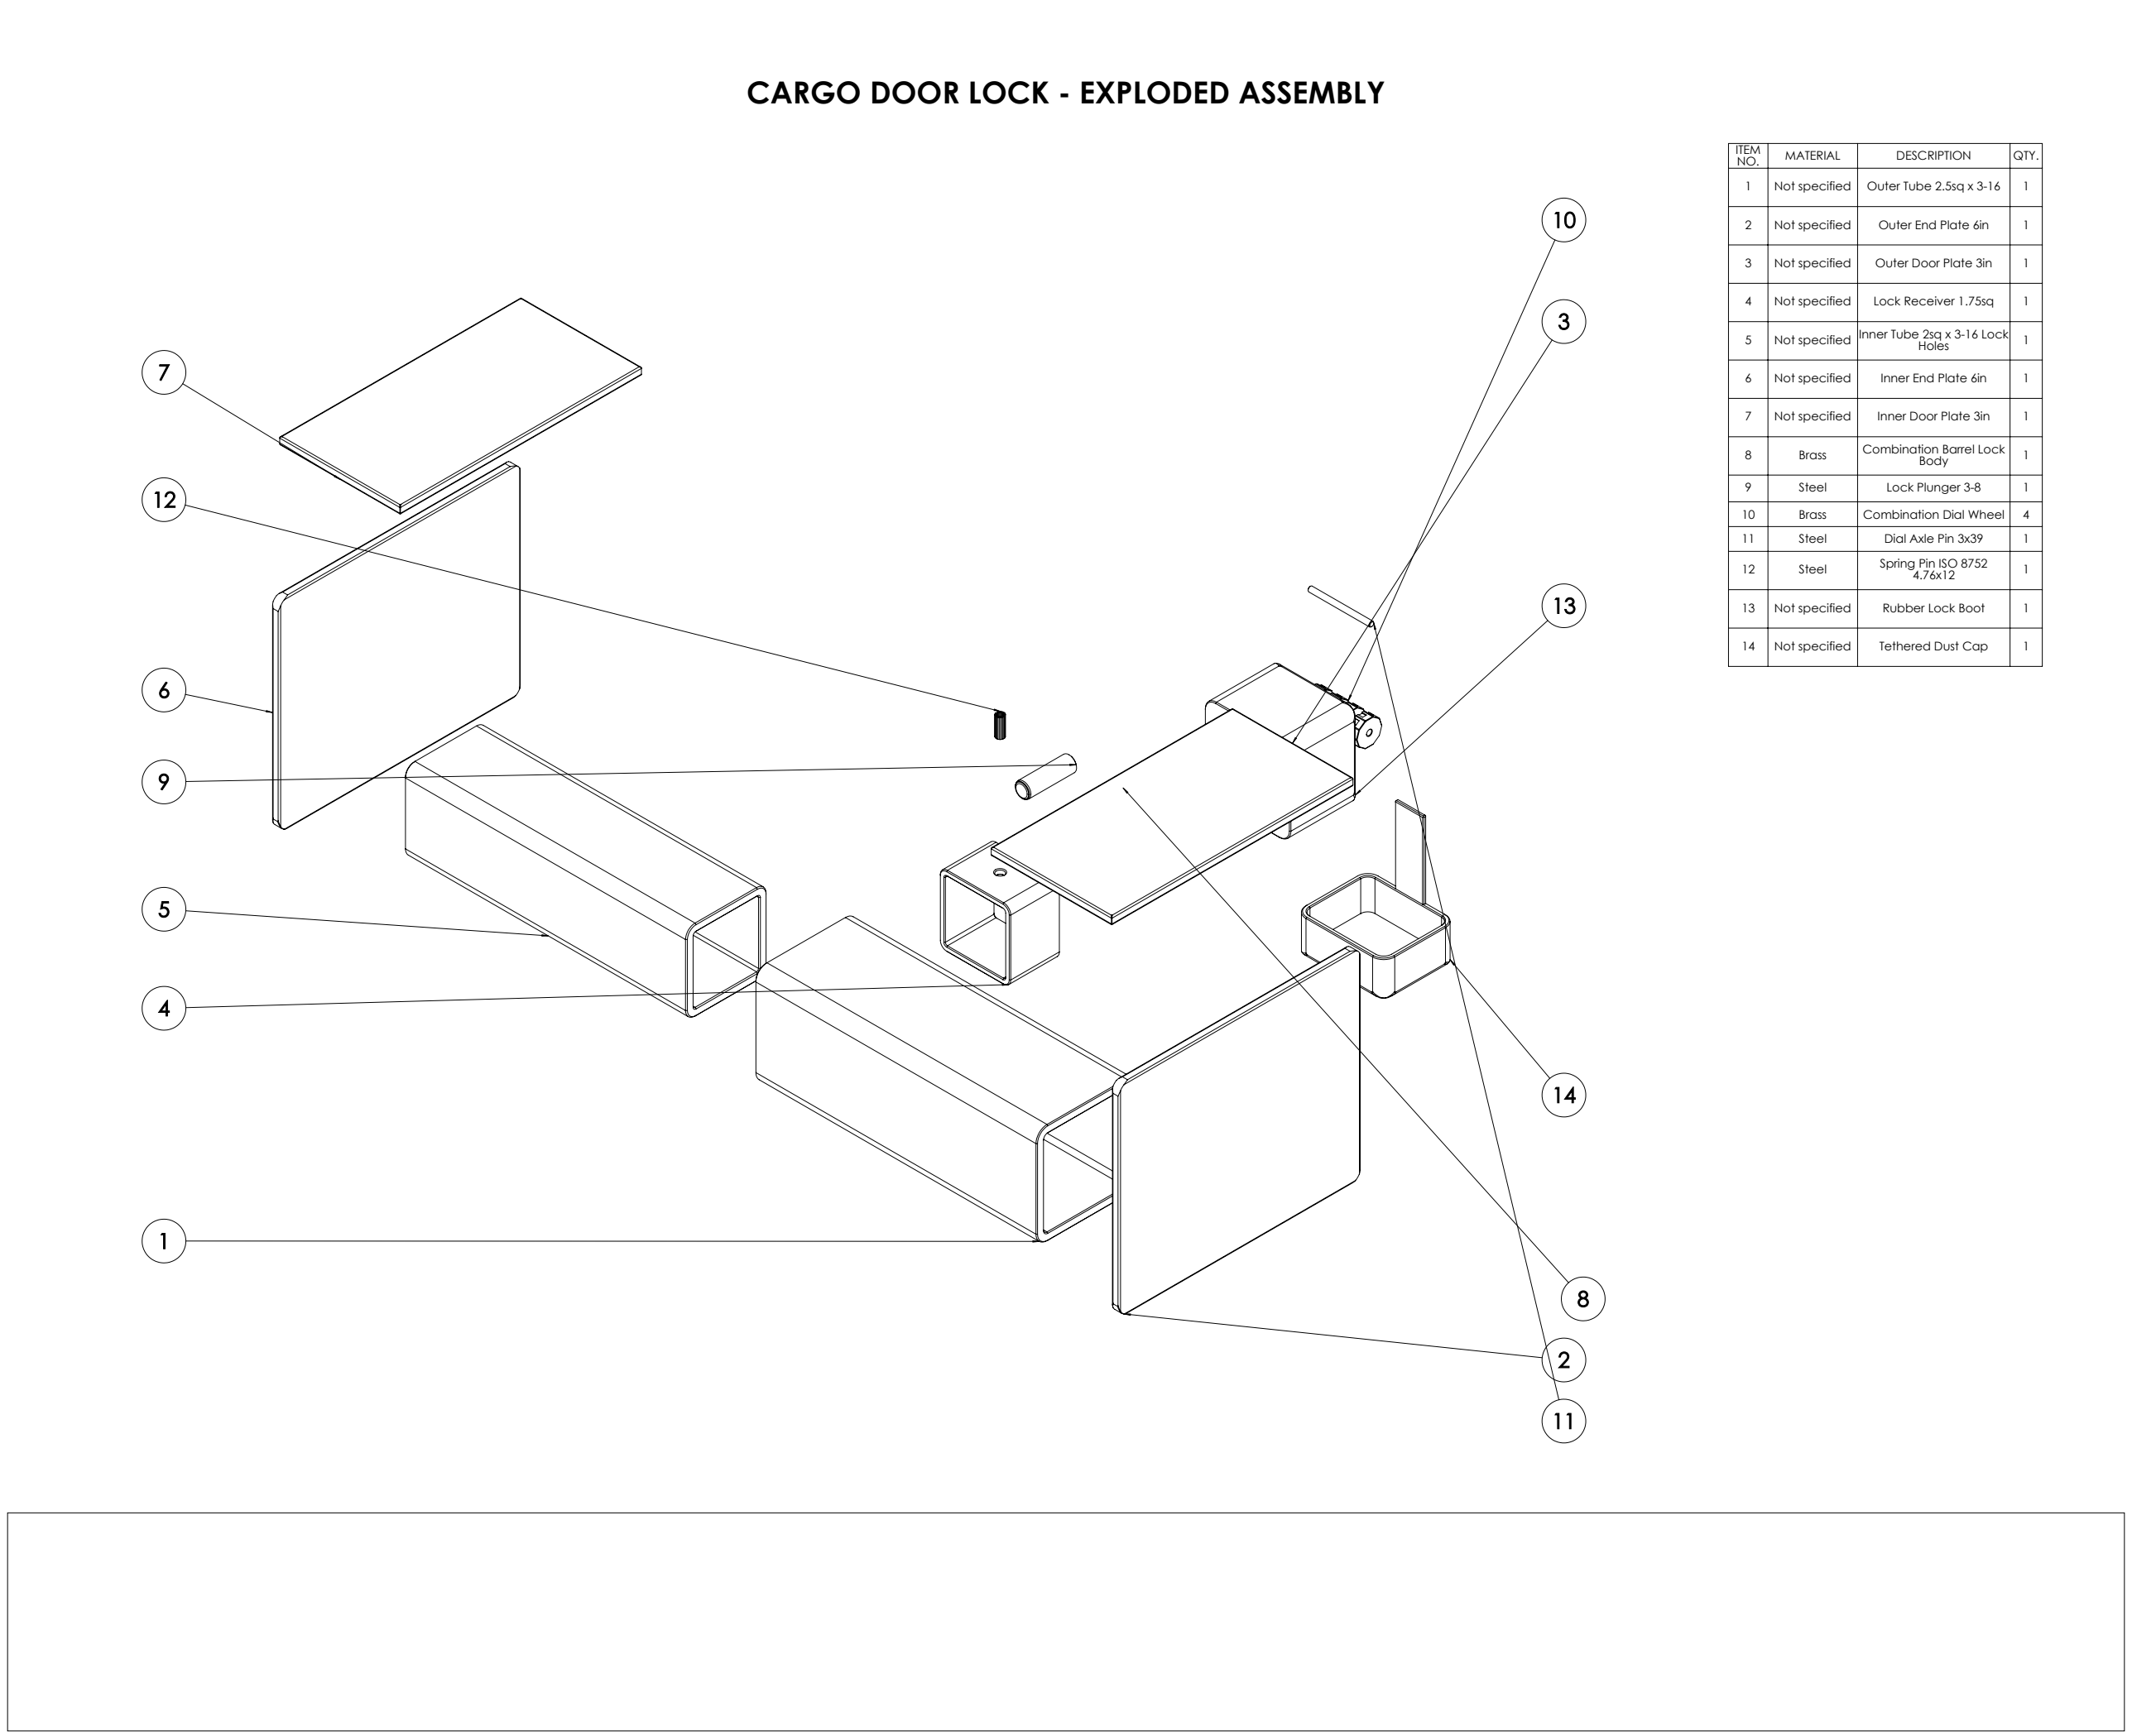
ISO-10303-21;
HEADER;
/* Generated by software containing ST-Developer
 * from STEP Tools, Inc. (www.steptools.com) 
 */

FILE_DESCRIPTION(
/* description */ (''),
/* implementation_level */ '2;1');

FILE_NAME(
/* name */ 'MAS-499',
/* time_stamp */ '2026-10-25T01:30:15-07:00',
/* author */ (''),
/* organization */ (''),
/* preprocessor_version */ 'ST-DEVELOPER v20.2',
/* originating_system */ 'Autodesk Translation Framework v15.15.0.0',
/* authorisation */ '');

FILE_SCHEMA (('AUTOMOTIVE_DESIGN { 1 0 10303 214 3 1 1 }'));
ENDSEC;

DATA;
#10=MECHANICAL_DESIGN_GEOMETRIC_PRESENTATION_REPRESENTATION('',(#563,#564,
#565,#566,#567,#568,#569,#570,#571,#572,#573,#574,#575,#576),#32309);
#11=ITEM_DEFINED_TRANSFORMATION($,$,#13974,#14987);
#12=ITEM_DEFINED_TRANSFORMATION($,$,#14060,#14988);
#13=ITEM_DEFINED_TRANSFORMATION($,$,#14095,#14989);
#14=ITEM_DEFINED_TRANSFORMATION($,$,#14114,#14990);
#15=ITEM_DEFINED_TRANSFORMATION($,$,#14204,#14991);
#16=ITEM_DEFINED_TRANSFORMATION($,$,#14378,#14992);
#17=ITEM_DEFINED_TRANSFORMATION($,$,#14413,#14993);
#18=ITEM_DEFINED_TRANSFORMATION($,$,#14432,#14994);
#19=ITEM_DEFINED_TRANSFORMATION($,$,#14610,#14995);
#20=ITEM_DEFINED_TRANSFORMATION($,$,#14627,#14996);
#21=ITEM_DEFINED_TRANSFORMATION($,$,#14637,#14997);
#22=ITEM_DEFINED_TRANSFORMATION($,$,#14690,#14998);
#23=ITEM_DEFINED_TRANSFORMATION($,$,#14802,#14999);
#24=ITEM_DEFINED_TRANSFORMATION($,$,#14889,#15000);
#25=ITEM_DEFINED_TRANSFORMATION($,$,#14889,#15001);
#26=ITEM_DEFINED_TRANSFORMATION($,$,#14889,#15002);
#27=ITEM_DEFINED_TRANSFORMATION($,$,#14889,#15003);
#28=(
REPRESENTATION_RELATIONSHIP($,$,#32362,#32361)
REPRESENTATION_RELATIONSHIP_WITH_TRANSFORMATION(#11)
SHAPE_REPRESENTATION_RELATIONSHIP()
);
#29=(
REPRESENTATION_RELATIONSHIP($,$,#32363,#32361)
REPRESENTATION_RELATIONSHIP_WITH_TRANSFORMATION(#12)
SHAPE_REPRESENTATION_RELATIONSHIP()
);
#30=(
REPRESENTATION_RELATIONSHIP($,$,#32364,#32361)
REPRESENTATION_RELATIONSHIP_WITH_TRANSFORMATION(#13)
SHAPE_REPRESENTATION_RELATIONSHIP()
);
#31=(
REPRESENTATION_RELATIONSHIP($,$,#32365,#32361)
REPRESENTATION_RELATIONSHIP_WITH_TRANSFORMATION(#14)
SHAPE_REPRESENTATION_RELATIONSHIP()
);
#32=(
REPRESENTATION_RELATIONSHIP($,$,#32366,#32361)
REPRESENTATION_RELATIONSHIP_WITH_TRANSFORMATION(#15)
SHAPE_REPRESENTATION_RELATIONSHIP()
);
#33=(
REPRESENTATION_RELATIONSHIP($,$,#32367,#32361)
REPRESENTATION_RELATIONSHIP_WITH_TRANSFORMATION(#16)
SHAPE_REPRESENTATION_RELATIONSHIP()
);
#34=(
REPRESENTATION_RELATIONSHIP($,$,#32368,#32361)
REPRESENTATION_RELATIONSHIP_WITH_TRANSFORMATION(#17)
SHAPE_REPRESENTATION_RELATIONSHIP()
);
#35=(
REPRESENTATION_RELATIONSHIP($,$,#32369,#32361)
REPRESENTATION_RELATIONSHIP_WITH_TRANSFORMATION(#18)
SHAPE_REPRESENTATION_RELATIONSHIP()
);
#36=(
REPRESENTATION_RELATIONSHIP($,$,#32370,#32361)
REPRESENTATION_RELATIONSHIP_WITH_TRANSFORMATION(#19)
SHAPE_REPRESENTATION_RELATIONSHIP()
);
#37=(
REPRESENTATION_RELATIONSHIP($,$,#32371,#32361)
REPRESENTATION_RELATIONSHIP_WITH_TRANSFORMATION(#20)
SHAPE_REPRESENTATION_RELATIONSHIP()
);
#38=(
REPRESENTATION_RELATIONSHIP($,$,#32372,#32361)
REPRESENTATION_RELATIONSHIP_WITH_TRANSFORMATION(#21)
SHAPE_REPRESENTATION_RELATIONSHIP()
);
#39=(
REPRESENTATION_RELATIONSHIP($,$,#32373,#32361)
REPRESENTATION_RELATIONSHIP_WITH_TRANSFORMATION(#22)
SHAPE_REPRESENTATION_RELATIONSHIP()
);
#40=(
REPRESENTATION_RELATIONSHIP($,$,#32374,#32361)
REPRESENTATION_RELATIONSHIP_WITH_TRANSFORMATION(#23)
SHAPE_REPRESENTATION_RELATIONSHIP()
);
#41=(
REPRESENTATION_RELATIONSHIP($,$,#32375,#32361)
REPRESENTATION_RELATIONSHIP_WITH_TRANSFORMATION(#24)
SHAPE_REPRESENTATION_RELATIONSHIP()
);
#42=(
REPRESENTATION_RELATIONSHIP($,$,#32375,#32361)
REPRESENTATION_RELATIONSHIP_WITH_TRANSFORMATION(#25)
SHAPE_REPRESENTATION_RELATIONSHIP()
);
#43=(
REPRESENTATION_RELATIONSHIP($,$,#32375,#32361)
REPRESENTATION_RELATIONSHIP_WITH_TRANSFORMATION(#26)
SHAPE_REPRESENTATION_RELATIONSHIP()
);
#44=(
REPRESENTATION_RELATIONSHIP($,$,#32375,#32361)
REPRESENTATION_RELATIONSHIP_WITH_TRANSFORMATION(#27)
SHAPE_REPRESENTATION_RELATIONSHIP()
);
#45=CONTEXT_DEPENDENT_SHAPE_REPRESENTATION(#28,#32344);
#46=CONTEXT_DEPENDENT_SHAPE_REPRESENTATION(#29,#32345);
#47=CONTEXT_DEPENDENT_SHAPE_REPRESENTATION(#30,#32346);
#48=CONTEXT_DEPENDENT_SHAPE_REPRESENTATION(#31,#32347);
#49=CONTEXT_DEPENDENT_SHAPE_REPRESENTATION(#32,#32348);
#50=CONTEXT_DEPENDENT_SHAPE_REPRESENTATION(#33,#32349);
#51=CONTEXT_DEPENDENT_SHAPE_REPRESENTATION(#34,#32350);
#52=CONTEXT_DEPENDENT_SHAPE_REPRESENTATION(#35,#32351);
#53=CONTEXT_DEPENDENT_SHAPE_REPRESENTATION(#36,#32352);
#54=CONTEXT_DEPENDENT_SHAPE_REPRESENTATION(#37,#32353);
#55=CONTEXT_DEPENDENT_SHAPE_REPRESENTATION(#38,#32354);
#56=CONTEXT_DEPENDENT_SHAPE_REPRESENTATION(#39,#32355);
#57=CONTEXT_DEPENDENT_SHAPE_REPRESENTATION(#40,#32356);
#58=CONTEXT_DEPENDENT_SHAPE_REPRESENTATION(#41,#32357);
#59=CONTEXT_DEPENDENT_SHAPE_REPRESENTATION(#42,#32358);
#60=CONTEXT_DEPENDENT_SHAPE_REPRESENTATION(#43,#32359);
#61=CONTEXT_DEPENDENT_SHAPE_REPRESENTATION(#44,#32360);
#62=NEXT_ASSEMBLY_USAGE_OCCURRENCE('01_Outer_Tube_2.5sq_x_3-16:2',
'01_Outer_Tube_2.5sq_x_3-16:2','01_Outer_Tube_2.5sq_x_3-16:2',#32377,#32378,
'01_Outer_Tube_2.5sq_x_3-16:2');
#63=NEXT_ASSEMBLY_USAGE_OCCURRENCE('02_Outer_End_Plate_6in:2',
'02_Outer_End_Plate_6in:2','02_Outer_End_Plate_6in:2',#32377,#32379,
'02_Outer_End_Plate_6in:2');
#64=NEXT_ASSEMBLY_USAGE_OCCURRENCE('03_Outer_Door_Plate_3in:2',
'03_Outer_Door_Plate_3in:2','03_Outer_Door_Plate_3in:2',#32377,#32380,
'03_Outer_Door_Plate_3in:2');
#65=NEXT_ASSEMBLY_USAGE_OCCURRENCE('04_Lock_Receiver_1.75sq:2',
'04_Lock_Receiver_1.75sq:2','04_Lock_Receiver_1.75sq:2',#32377,#32381,
'04_Lock_Receiver_1.75sq:2');
#66=NEXT_ASSEMBLY_USAGE_OCCURRENCE(
'05_Inner_Tube_2sq_x_3-16_Lock_Holes:2',
'05_Inner_Tube_2sq_x_3-16_Lock_Holes:2',
'05_Inner_Tube_2sq_x_3-16_Lock_Holes:2',#32377,#32382,
'05_Inner_Tube_2sq_x_3-16_Lock_Holes:2');
#67=NEXT_ASSEMBLY_USAGE_OCCURRENCE('06_Inner_End_Plate_6in:2',
'06_Inner_End_Plate_6in:2','06_Inner_End_Plate_6in:2',#32377,#32383,
'06_Inner_End_Plate_6in:2');
#68=NEXT_ASSEMBLY_USAGE_OCCURRENCE('07_Inner_Door_Plate_3in:2',
'07_Inner_Door_Plate_3in:2','07_Inner_Door_Plate_3in:2',#32377,#32384,
'07_Inner_Door_Plate_3in:2');
#69=NEXT_ASSEMBLY_USAGE_OCCURRENCE('08_Combination_Barrel_Lock_Body:2',
'08_Combination_Barrel_Lock_Body:2','08_Combination_Barrel_Lock_Body:2',
#32377,#32385,'08_Combination_Barrel_Lock_Body:2');
#70=NEXT_ASSEMBLY_USAGE_OCCURRENCE('09_Lock_Plunger_3-8:2',
'09_Lock_Plunger_3-8:2','09_Lock_Plunger_3-8:2',#32377,#32386,
'09_Lock_Plunger_3-8:2');
#71=NEXT_ASSEMBLY_USAGE_OCCURRENCE('11_Dial_Axle_Pin_3x39:2',
'11_Dial_Axle_Pin_3x39:2','11_Dial_Axle_Pin_3x39:2',#32377,#32387,
'11_Dial_Axle_Pin_3x39:2');
#72=NEXT_ASSEMBLY_USAGE_OCCURRENCE('12_Spring_Pin_ISO_8752_4.76x12:2',
'12_Spring_Pin_ISO_8752_4.76x12:2','12_Spring_Pin_ISO_8752_4.76x12:2',#32377,
#32388,'12_Spring_Pin_ISO_8752_4.76x12:2');
#73=NEXT_ASSEMBLY_USAGE_OCCURRENCE('13_Rubber_Lock_Boot:2',
'13_Rubber_Lock_Boot:2','13_Rubber_Lock_Boot:2',#32377,#32389,
'13_Rubber_Lock_Boot:2');
#74=NEXT_ASSEMBLY_USAGE_OCCURRENCE('14_Tethered_Dust_Cap:2',
'14_Tethered_Dust_Cap:2','14_Tethered_Dust_Cap:2',#32377,#32390,
'14_Tethered_Dust_Cap:2');
#75=NEXT_ASSEMBLY_USAGE_OCCURRENCE('10_Combination_Dial_Wheel:2',
'10_Combination_Dial_Wheel:2','10_Combination_Dial_Wheel:2',#32377,#32391,
'10_Combination_Dial_Wheel:2');
#76=NEXT_ASSEMBLY_USAGE_OCCURRENCE('10_Combination_Dial_Wheel:3',
'10_Combination_Dial_Wheel:3','10_Combination_Dial_Wheel:3',#32377,#32391,
'10_Combination_Dial_Wheel:3');
#77=NEXT_ASSEMBLY_USAGE_OCCURRENCE('10_Combination_Dial_Wheel:4',
'10_Combination_Dial_Wheel:4','10_Combination_Dial_Wheel:4',#32377,#32391,
'10_Combination_Dial_Wheel:4');
#78=NEXT_ASSEMBLY_USAGE_OCCURRENCE('10_Combination_Dial_Wheel:5',
'10_Combination_Dial_Wheel:5','10_Combination_Dial_Wheel:5',#32377,#32391,
'10_Combination_Dial_Wheel:5');
#79=ELLIPSE('',#14443,12.7279220613578,8.99999999999999);
#80=ELLIPSE('',#14447,12.7279220613579,9.);
#81=ELLIPSE('',#14470,12.7279220613578,9.);
#82=ELLIPSE('',#14474,12.7279220613578,9.);
#83=(
BOUNDED_CURVE()
B_SPLINE_CURVE(2,(#25941,#25942,#25943),.UNSPECIFIED.,.F.,.F.)
B_SPLINE_CURVE_WITH_KNOTS((3,3),(0.,0.083454512499127),.UNSPECIFIED.)
CURVE()
GEOMETRIC_REPRESENTATION_ITEM()
RATIONAL_B_SPLINE_CURVE((1.,1.00072968826169,1.))
REPRESENTATION_ITEM('')
);
#84=(
BOUNDED_CURVE()
B_SPLINE_CURVE(2,(#25958,#25959,#25960),.UNSPECIFIED.,.F.,.F.)
B_SPLINE_CURVE_WITH_KNOTS((3,3),(0.,0.0834545124991277),.UNSPECIFIED.)
CURVE()
GEOMETRIC_REPRESENTATION_ITEM()
RATIONAL_B_SPLINE_CURVE((1.,1.00072968826163,1.))
REPRESENTATION_ITEM('')
);
#85=(
BOUNDED_CURVE()
B_SPLINE_CURVE(2,(#26021,#26022,#26023),.UNSPECIFIED.,.F.,.F.)
B_SPLINE_CURVE_WITH_KNOTS((3,3),(0.,0.0834545124991279),.UNSPECIFIED.)
CURVE()
GEOMETRIC_REPRESENTATION_ITEM()
RATIONAL_B_SPLINE_CURVE((1.,1.00072968826024,1.))
REPRESENTATION_ITEM('')
);
#86=(
BOUNDED_CURVE()
B_SPLINE_CURVE(2,(#26038,#26039,#26040),.UNSPECIFIED.,.F.,.F.)
B_SPLINE_CURVE_WITH_KNOTS((3,3),(0.,0.083454512499128),.UNSPECIFIED.)
CURVE()
GEOMETRIC_REPRESENTATION_ITEM()
RATIONAL_B_SPLINE_CURVE((1.,1.0007296882565,1.))
REPRESENTATION_ITEM('')
);
#87=(
BOUNDED_CURVE()
B_SPLINE_CURVE(3,(#30768,#30769,#30770,#30771,#30772,#30773,#30774,#30775,
#30776,#30777,#30778,#30779),.UNSPECIFIED.,.F.,.F.)
B_SPLINE_CURVE_WITH_KNOTS((4,2,2,2,2,4),(0.000100085581199306,0.11804875878528,
0.236101413685198,0.384034650166034,0.497829447458985,0.511841573844537),
 .UNSPECIFIED.)
CURVE()
GEOMETRIC_REPRESENTATION_ITEM()
RATIONAL_B_SPLINE_CURVE((1.,1.,1.,1.,1.,1.,1.,1.,1.,1.,1.,1.))
REPRESENTATION_ITEM('')
);
#88=B_SPLINE_CURVE_WITH_KNOTS('',3,(#18634,#18635,#18636,#18637,#18638,
#18639,#18640,#18641,#18642,#18643,#18644,#18645,#18646,#18647,#18648,#18649,
#18650,#18651,#18652,#18653,#18654,#18655,#18656,#18657,#18658,#18659,#18660,
#18661,#18662,#18663,#18664,#18665,#18666,#18667,#18668,#18669,#18670,#18671,
#18672,#18673,#18674,#18675,#18676,#18677,#18678,#18679,#18680,#18681,#18682,
#18683,#18684,#18685,#18686,#18687,#18688,#18689,#18690,#18691,#18692,#18693,
#18694,#18695,#18696,#18697,#18698,#18699,#18700,#18701,#18702,#18703,#18704,
#18705,#18706,#18707,#18708,#18709,#18710,#18711,#18712,#18713,#18714,#18715),
 .UNSPECIFIED.,.F.,.F.,(4,3,3,3,3,3,3,3,3,3,3,3,3,3,3,3,3,3,3,3,3,3,3,3,
3,3,3,4),(0.,0.0295705059520471,0.06051594873034,0.0926038163611335,0.126139587235275,
0.161619669140697,0.19997110729461,0.243460414926569,0.31097643988682,0.354040412393894,
0.394412886619275,0.429686040742309,0.462833625340497,0.494651029781358,
0.527129557828368,0.560643520110525,0.596019930687279,0.634095034705998,
0.676984118479283,0.757738088859462,0.799051739150417,0.836280907609681,
0.871099049046634,0.903485295335691,0.934889314251083,0.965468175632905,
0.995091329104342,1.),.UNSPECIFIED.);
#89=B_SPLINE_CURVE_WITH_KNOTS('',3,(#18717,#18718,#18719,#18720),
 .UNSPECIFIED.,.F.,.F.,(4,4),(-1.,0.),.UNSPECIFIED.);
#90=B_SPLINE_CURVE_WITH_KNOTS('',3,(#18722,#18723,#18724,#18725,#18726,
#18727,#18728,#18729,#18730,#18731,#18732,#18733,#18734,#18735,#18736,#18737,
#18738,#18739,#18740,#18741,#18742,#18743,#18744,#18745,#18746,#18747,#18748,
#18749,#18750,#18751,#18752,#18753,#18754,#18755,#18756,#18757,#18758,#18759,
#18760,#18761,#18762,#18763,#18764,#18765,#18766,#18767,#18768,#18769,#18770,
#18771,#18772,#18773),.UNSPECIFIED.,.F.,.F.,(4,3,3,3,3,3,3,3,3,3,3,3,3,
3,3,3,3,4),(0.,0.0499444618814776,0.102213228769125,0.161337745851018,0.226027786935006,
0.32277431356813,0.388018393772404,0.444871191794535,0.498045966144255,
0.551308035192963,0.608971249854249,0.676370629164652,0.757277971873489,
0.819640070739892,0.87628793152519,0.929442915859961,0.979183143018599,
1.),.UNSPECIFIED.);
#91=B_SPLINE_CURVE_WITH_KNOTS('',3,(#18813,#18814,#18815,#18816,#18817,
#18818,#18819,#18820,#18821,#18822,#18823,#18824,#18825,#18826,#18827,#18828,
#18829,#18830,#18831,#18832,#18833,#18834,#18835,#18836,#18837,#18838,#18839,
#18840,#18841,#18842,#18843,#18844,#18845,#18846,#18847,#18848,#18849,#18850,
#18851,#18852,#18853,#18854,#18855,#18856,#18857,#18858,#18859,#18860,#18861,
#18862,#18863,#18864),.UNSPECIFIED.,.F.,.F.,(4,3,3,3,3,3,3,3,3,3,3,3,3,
3,3,3,3,4),(0.,0.0499441833889704,0.102212663354794,0.161336814770105,0.226026300658832,
0.322773013076478,0.388016980146257,0.444869605985199,0.498043900535364,
0.551305760953485,0.608968431114082,0.676366602896629,0.757274952172472,
0.819637092644588,0.876284888158847,0.929439770312476,0.979179831895377,
1.),.UNSPECIFIED.);
#92=B_SPLINE_CURVE_WITH_KNOTS('',3,(#18866,#18867,#18868,#18869),
 .UNSPECIFIED.,.F.,.F.,(4,4),(0.,1.),.UNSPECIFIED.);
#93=B_SPLINE_CURVE_WITH_KNOTS('',3,(#18871,#18872,#18873,#18874,#18875,
#18876,#18877,#18878,#18879,#18880,#18881,#18882,#18883,#18884,#18885,#18886,
#18887,#18888,#18889,#18890,#18891,#18892,#18893,#18894,#18895,#18896,#18897,
#18898,#18899,#18900,#18901,#18902,#18903,#18904,#18905,#18906,#18907,#18908,
#18909,#18910,#18911,#18912,#18913,#18914,#18915,#18916,#18917,#18918,#18919,
#18920,#18921,#18922,#18923,#18924,#18925,#18926,#18927,#18928,#18929,#18930,
#18931,#18932,#18933,#18934,#18935,#18936,#18937,#18938,#18939,#18940,#18941,
#18942,#18943,#18944,#18945,#18946,#18947,#18948,#18949,#18950,#18951,#18952),
 .UNSPECIFIED.,.F.,.F.,(4,3,3,3,3,3,3,3,3,3,3,3,3,3,3,3,3,3,3,3,3,3,3,3,
3,3,3,4),(0.,0.0295773880527055,0.0605304168417959,0.0926266477934975,0.12617192252577,
0.16166335905183,0.200029751866471,0.243548698202303,0.31096188049889,0.354026762967709,
0.394400090282227,0.429679987033159,0.462839402284378,0.494661356434203,
0.527132671759088,0.560640873791091,0.596011156294116,0.634079510048534,
0.676959318035126,0.757719488526345,0.799022961860359,0.836244255344789,
0.871055470881663,0.903435211406727,0.934833076384915,0.965406058046024,
0.995023143022087,1.),.UNSPECIFIED.);
#94=B_SPLINE_CURVE_WITH_KNOTS('',3,(#18979,#18980,#18981,#18982,#18983,
#18984),.UNSPECIFIED.,.F.,.F.,(4,2,4),(9.99629094513137E-5,0.155241085196768,
0.273153287835105),.UNSPECIFIED.);
#95=B_SPLINE_CURVE_WITH_KNOTS('',3,(#18987,#18988,#18989,#18990,#18991,
#18992),.UNSPECIFIED.,.F.,.F.,(4,2,4),(-0.273153287835105,-0.155241085196768,
-9.99629094513137E-5),.UNSPECIFIED.);
#96=B_SPLINE_CURVE_WITH_KNOTS('',3,(#19018,#19019,#19020,#19021),
 .UNSPECIFIED.,.F.,.F.,(4,4),(-0.310482170393534,-0.273153287835093),
 .UNSPECIFIED.);
#97=B_SPLINE_CURVE_WITH_KNOTS('',3,(#19022,#19023,#19024,#19025),
 .UNSPECIFIED.,.F.,.F.,(4,4),(0.273153287835093,0.310482170393534),
 .UNSPECIFIED.);
#98=B_SPLINE_CURVE_WITH_KNOTS('',3,(#19051,#19052,#19053,#19054,#19055,
#19056),.UNSPECIFIED.,.F.,.F.,(4,2,4),(-0.954291288267864,-0.799150016166132,
-0.681237813527798),.UNSPECIFIED.);
#99=B_SPLINE_CURVE_WITH_KNOTS('',3,(#19059,#19060,#19061,#19062,#19063,
#19064),.UNSPECIFIED.,.F.,.F.,(4,2,4),(0.681237813527798,0.799150016166132,
0.954291288267864),.UNSPECIFIED.);
#100=B_SPLINE_CURVE_WITH_KNOTS('',3,(#19081,#19082,#19083,#19084),
 .UNSPECIFIED.,.F.,.F.,(4,4),(-0.681237813527811,-0.643908930969367),
 .UNSPECIFIED.);
#101=B_SPLINE_CURVE_WITH_KNOTS('',3,(#19085,#19086,#19087,#19088),
 .UNSPECIFIED.,.F.,.F.,(4,4),(0.643908930969367,0.681237813527811),
 .UNSPECIFIED.);
#102=B_SPLINE_CURVE_WITH_KNOTS('',3,(#19093,#19094,#19095,#19096,#19097,
#19098,#19099,#19100,#19101,#19102,#19103,#19104,#19105,#19106,#19107,#19108,
#19109,#19110,#19111,#19112,#19113,#19114,#19115,#19116,#19117,#19118,#19119,
#19120,#19121,#19122,#19123,#19124,#19125,#19126,#19127,#19128,#19129,#19130,
#19131,#19132,#19133,#19134,#19135,#19136,#19137,#19138,#19139,#19140,#19141,
#19142,#19143,#19144,#19145,#19146,#19147,#19148,#19149,#19150,#19151,#19152,
#19153,#19154,#19155,#19156,#19157,#19158,#19159,#19160,#19161,#19162,#19163,
#19164,#19165,#19166,#19167,#19168,#19169,#19170,#19171,#19172,#19173,#19174),
 .UNSPECIFIED.,.F.,.F.,(4,3,3,3,3,3,3,3,3,3,3,3,3,3,3,3,3,3,3,3,3,3,3,3,
3,3,3,4),(0.,0.0295773880962405,0.0605304169310475,0.0926266479315681,0.126171922717038,
0.161663359303526,0.200029752189728,0.243548698625291,0.310961878288235,
0.35402676089522,0.394400088339269,0.429679985266982,0.462839400402085,
0.494661354749945,0.527132670284999,0.560640872291038,0.596011154748267,
0.634079508418766,0.676959316170582,0.757719487127936,0.79902296069953,
0.836244254323238,0.871055469962877,0.903435210560169,0.9348330756024,0.965406057321837,
0.995023142345411,1.),.UNSPECIFIED.);
#103=B_SPLINE_CURVE_WITH_KNOTS('',3,(#19176,#19177,#19178,#19179,#19180,
#19181),.UNSPECIFIED.,.F.,.F.,(4,2,4),(-0.273153287835103,-0.155241085196768,
-9.99629094513097E-5),.UNSPECIFIED.);
#104=B_SPLINE_CURVE_WITH_KNOTS('',3,(#19199,#19200,#19201,#19202,#19203,
#19204,#19205,#19206,#19207,#19208,#19209,#19210,#19211,#19212,#19213,#19214,
#19215,#19216,#19217,#19218,#19219,#19220,#19221,#19222,#19223,#19224,#19225,
#19226,#19227,#19228,#19229,#19230,#19231,#19232,#19233,#19234,#19235,#19236,
#19237,#19238,#19239,#19240,#19241,#19242,#19243,#19244,#19245,#19246,#19247,
#19248,#19249,#19250),.UNSPECIFIED.,.F.,.F.,(4,3,3,3,3,3,3,3,3,3,3,3,3,
3,3,3,3,4),(0.,0.0499444622917576,0.102213229604467,0.161337747231124,0.226027789147348,
0.32277431550393,0.388018395851454,0.444871194115429,0.498045969164268,
0.551308038550752,0.608971254052268,0.676370635217512,0.757277976413134,
0.81964007522294,0.876287936115381,0.929442920613543,0.979183148031846,
1.),.UNSPECIFIED.);
#105=B_SPLINE_CURVE_WITH_KNOTS('',3,(#19252,#19253,#19254,#19255,#19256,
#19257),.UNSPECIFIED.,.F.,.F.,(4,2,4),(0.681229980645395,0.79914218328373,
0.954283455385462),.UNSPECIFIED.);
#106=B_SPLINE_CURVE_WITH_KNOTS('',3,(#19259,#19260,#19261,#19262),
 .UNSPECIFIED.,.F.,.F.,(4,4),(0.643901098086962,0.681229980645409),
 .UNSPECIFIED.);
#107=B_SPLINE_CURVE_WITH_KNOTS('',3,(#19266,#19267,#19268,#19269),
 .UNSPECIFIED.,.F.,.F.,(4,4),(0.269588855200382,0.305932679404608),
 .UNSPECIFIED.);
#108=B_SPLINE_CURVE_WITH_KNOTS('',3,(#19271,#19272,#19273,#19274,#19275,
#19276),.UNSPECIFIED.,.F.,.F.,(4,2,4),(9.97881403247492E-5,0.166940126137213,
0.269588855200419),.UNSPECIFIED.);
#109=B_SPLINE_CURVE_WITH_KNOTS('',3,(#19277,#19278,#19279,#19280,#19281,
#19282,#19283,#19284,#19285,#19286,#19287,#19288,#19289,#19290,#19291,#19292,
#19293,#19294,#19295,#19296,#19297,#19298,#19299,#19300,#19301,#19302,#19303,
#19304,#19305,#19306,#19307,#19308,#19309,#19310,#19311,#19312,#19313,#19314,
#19315,#19316,#19317,#19318,#19319,#19320,#19321,#19322,#19323,#19324,#19325,
#19326,#19327,#19328),.UNSPECIFIED.,.F.,.F.,(4,3,3,3,3,3,3,3,3,3,3,3,3,
3,3,3,3,4),(0.,0.0499444877726433,0.102213281220285,0.161337835137364,0.226027936148337,
0.322774444129795,0.38801851522186,0.444871319243691,0.498046130430203,
0.551308243614294,0.608971537556607,0.676371082027953,0.757278311520965,
0.819640416091138,0.876288295150041,0.92944330183216,0.979183558774527,
1.),.UNSPECIFIED.);
#110=B_SPLINE_CURVE_WITH_KNOTS('',3,(#19351,#19352,#19353,#19354,#19355,
#19356,#19357,#19358,#19359,#19360,#19361,#19362,#19363,#19364,#19365,#19366,
#19367,#19368,#19369,#19370,#19371,#19372,#19373,#19374,#19375,#19376,#19377,
#19378,#19379,#19380,#19381,#19382,#19383,#19384,#19385,#19386,#19387,#19388,
#19389,#19390,#19391,#19392,#19393,#19394,#19395,#19396,#19397,#19398,#19399,
#19400,#19401,#19402,#19403,#19404,#19405,#19406,#19407,#19408,#19409,#19410,
#19411,#19412,#19413,#19414,#19415,#19416,#19417,#19418,#19419,#19420,#19421,
#19422,#19423,#19424,#19425,#19426,#19427,#19428,#19429,#19430,#19431,#19432),
 .UNSPECIFIED.,.F.,.F.,(4,3,3,3,3,3,3,3,3,3,3,3,3,3,3,3,3,3,3,3,3,3,3,3,
3,3,3,4),(0.,0.0295705062457886,0.0605159494602176,0.0926038176850879,0.126139589401718,
0.161619672576972,0.199971112846056,0.243460425882021,0.310976395562794,
0.35404037084012,0.394412847662612,0.429686002557242,0.462833578893964,
0.494650986322964,0.527129524428408,0.560643490399518,0.596019903970715,
0.634095009431096,0.67698408832498,0.757738066243735,0.799051737694099,
0.836280920233922,0.87109907297074,0.903485328812536,0.934889356536429,
0.965468226164381,0.995091387717599,1.),.UNSPECIFIED.);
#111=B_SPLINE_CURVE_WITH_KNOTS('',3,(#19434,#19435,#19436,#19437),
 .UNSPECIFIED.,.F.,.F.,(4,4),(-1.,0.),.UNSPECIFIED.);
#112=B_SPLINE_CURVE_WITH_KNOTS('',3,(#19439,#19440,#19441,#19442,#19443,
#19444,#19445,#19446,#19447,#19448,#19449,#19450,#19451,#19452,#19453,#19454,
#19455,#19456,#19457,#19458,#19459,#19460,#19461,#19462,#19463,#19464,#19465,
#19466,#19467,#19468,#19469,#19470,#19471,#19472,#19473,#19474,#19475,#19476,
#19477,#19478,#19479,#19480,#19481,#19482,#19483,#19484,#19485,#19486,#19487,
#19488,#19489,#19490),.UNSPECIFIED.,.F.,.F.,(4,3,3,3,3,3,3,3,3,3,3,3,3,
3,3,3,3,4),(0.,0.049944493509105,0.102213293185184,0.161337852934914,0.226027959979003,
0.322774464981628,0.388018552338671,0.444871367106078,0.498046192643883,
0.551308282903018,0.608971555280469,0.676371064186631,0.757278298139973,
0.81964039022404,0.87628825630229,0.929443250152998,0.979183493767421,1.),
 .UNSPECIFIED.);
#113=B_SPLINE_CURVE_WITH_KNOTS('',3,(#19529,#19530,#19531,#19532,#19533,
#19534,#19535,#19536,#19537,#19538,#19539,#19540,#19541,#19542,#19543,#19544,
#19545,#19546,#19547,#19548,#19549,#19550,#19551,#19552,#19553,#19554,#19555,
#19556,#19557,#19558,#19559,#19560,#19561,#19562,#19563,#19564,#19565,#19566,
#19567,#19568,#19569,#19570,#19571,#19572,#19573,#19574,#19575,#19576,#19577,
#19578,#19579,#19580),.UNSPECIFIED.,.F.,.F.,(4,3,3,3,3,3,3,3,3,3,3,3,3,
3,3,3,3,4),(0.,0.0499441828918079,0.102212662342561,0.161336813097488,0.226026297979579,
0.322773010732132,0.388016977629376,0.444869603175185,0.498043896877559,
0.551305756885345,0.608968426026964,0.676366595561391,0.757274946671043,
0.819637087211295,0.876284882595595,0.929439764551152,0.979179825819233,
1.),.UNSPECIFIED.);
#114=B_SPLINE_CURVE_WITH_KNOTS('',3,(#19581,#19582,#19583,#19584),
 .UNSPECIFIED.,.F.,.F.,(4,4),(0.,1.),.UNSPECIFIED.);
#115=B_SPLINE_CURVE_WITH_KNOTS('',3,(#19610,#19611,#19612,#19613,#19614,
#19615),.UNSPECIFIED.,.F.,.F.,(4,2,4),(9.99629094513097E-5,0.155241085196768,
0.273153287835103),.UNSPECIFIED.);
#116=B_SPLINE_CURVE_WITH_KNOTS('',3,(#19642,#19643,#19644,#19645),
 .UNSPECIFIED.,.F.,.F.,(4,4),(-0.310482170393536,-0.273153287835089),
 .UNSPECIFIED.);
#117=B_SPLINE_CURVE_WITH_KNOTS('',3,(#19646,#19647,#19648,#19649),
 .UNSPECIFIED.,.F.,.F.,(4,4),(0.273153287835089,0.310482170393536),
 .UNSPECIFIED.);
#118=B_SPLINE_CURVE_WITH_KNOTS('',3,(#19675,#19676,#19677,#19678,#19679,
#19680),.UNSPECIFIED.,.F.,.F.,(4,2,4),(-0.945184496035906,-0.778344160365421,
-0.675695431302217),.UNSPECIFIED.);
#119=B_SPLINE_CURVE_WITH_KNOTS('',3,(#19683,#19684,#19685,#19686,#19687,
#19688),.UNSPECIFIED.,.F.,.F.,(4,2,4),(0.675695431302217,0.778344160365421,
0.945184496035906),.UNSPECIFIED.);
#120=B_SPLINE_CURVE_WITH_KNOTS('',3,(#19705,#19706,#19707,#19708),
 .UNSPECIFIED.,.F.,.F.,(4,4),(-0.675695431302254,-0.639351607098029),
 .UNSPECIFIED.);
#121=B_SPLINE_CURVE_WITH_KNOTS('',3,(#19709,#19710,#19711,#19712),
 .UNSPECIFIED.,.F.,.F.,(4,4),(0.639351607098029,0.675695431302254),
 .UNSPECIFIED.);
#122=B_SPLINE_CURVE_WITH_KNOTS('',3,(#19744,#19745,#19746,#19747,#19748,
#19749,#19750,#19751,#19752,#19753,#19754,#19755,#19756,#19757,#19758,#19759,
#19760,#19761,#19762,#19763,#19764,#19765,#19766,#19767,#19768,#19769,#19770,
#19771,#19772,#19773,#19774,#19775,#19776,#19777,#19778,#19779,#19780,#19781,
#19782,#19783,#19784,#19785,#19786,#19787,#19788,#19789,#19790,#19791,#19792,
#19793,#19794,#19795,#19796,#19797,#19798,#19799,#19800,#19801,#19802,#19803,
#19804,#19805,#19806,#19807,#19808,#19809,#19810,#19811,#19812,#19813,#19814,
#19815,#19816,#19817,#19818,#19819,#19820,#19821,#19822,#19823,#19824,#19825),
 .UNSPECIFIED.,.F.,.F.,(4,3,3,3,3,3,3,3,3,3,3,3,3,3,3,3,3,3,3,3,3,3,3,3,
3,3,3,4),(0.,0.0295705062009041,0.0605159493680217,0.0926038175409483,0.126139589200587,
0.161619672306982,0.199971112488613,0.243460425357206,0.310976394321422,
0.354040369676333,0.394412846571562,0.429686001479307,0.46283357764396,
0.49465098512599,0.527129523295935,0.560643489155532,0.596019902588203,
0.634095007862749,0.676984086399807,0.757738064799855,0.799051736386075,
0.836280918968163,0.871099071720543,0.903485327550832,0.934889355257872,
0.965468224868288,0.995091386390381,1.),.UNSPECIFIED.);
#123=B_SPLINE_CURVE_WITH_KNOTS('',3,(#19827,#19828,#19829,#19830),
 .UNSPECIFIED.,.F.,.F.,(4,4),(-1.,0.),.UNSPECIFIED.);
#124=B_SPLINE_CURVE_WITH_KNOTS('',3,(#19831,#19832,#19833,#19834,#19835,
#19836,#19837,#19838,#19839,#19840,#19841,#19842,#19843,#19844,#19845,#19846,
#19847,#19848,#19849,#19850,#19851,#19852,#19853,#19854,#19855,#19856,#19857,
#19858,#19859,#19860,#19861,#19862,#19863,#19864,#19865,#19866,#19867,#19868,
#19869,#19870,#19871,#19872,#19873,#19874,#19875,#19876,#19877,#19878,#19879,
#19880,#19881,#19882),.UNSPECIFIED.,.F.,.F.,(4,3,3,3,3,3,3,3,3,3,3,3,3,
3,3,3,3,4),(0.,0.0499444940857239,0.102213294358374,0.161337854873708,0.226027963088782,
0.322774467702684,0.388018555259764,0.444871370367514,0.498046196889068,
0.551308287624491,0.608971561184033,0.676371072696357,0.757278304522268,
0.819640396527144,0.87628826275593,0.92944325683678,0.979183500816116,1.),
 .UNSPECIFIED.);
#125=B_SPLINE_CURVE_WITH_KNOTS('',3,(#19921,#19922,#19923,#19924,#19925,
#19926,#19927,#19928,#19929,#19930,#19931,#19932,#19933,#19934,#19935,#19936,
#19937,#19938,#19939,#19940,#19941,#19942,#19943,#19944,#19945,#19946,#19947,
#19948,#19949,#19950,#19951,#19952,#19953,#19954,#19955,#19956,#19957,#19958,
#19959,#19960,#19961,#19962,#19963,#19964,#19965,#19966,#19967,#19968,#19969,
#19970,#19971,#19972),.UNSPECIFIED.,.F.,.F.,(4,3,3,3,3,3,3,3,3,3,3,3,3,
3,3,3,3,4),(0.,0.0499441826826897,0.102212661917196,0.161336812394391,0.22602629685116,
0.322773009744765,0.388016976569652,0.444869601991809,0.498043895337266,
0.551305755172809,0.608968423886568,0.676366592477159,0.757274944357869,
0.819637084926596,0.876284880256139,0.929439762127755,0.979179823263689,
1.),.UNSPECIFIED.);
#126=B_SPLINE_CURVE_WITH_KNOTS('',3,(#19974,#19975,#19976,#19977),
 .UNSPECIFIED.,.F.,.F.,(4,4),(0.,1.),.UNSPECIFIED.);
#127=B_SPLINE_CURVE_WITH_KNOTS('',3,(#19979,#19980,#19981,#19982,#19983,
#19984,#19985,#19986,#19987,#19988,#19989,#19990,#19991,#19992,#19993,#19994,
#19995,#19996,#19997,#19998,#19999,#20000,#20001,#20002,#20003,#20004,#20005,
#20006,#20007,#20008,#20009,#20010,#20011,#20012,#20013,#20014,#20015,#20016,
#20017,#20018,#20019,#20020,#20021,#20022,#20023,#20024,#20025,#20026,#20027,
#20028,#20029,#20030,#20031,#20032,#20033,#20034,#20035,#20036,#20037,#20038,
#20039,#20040,#20041,#20042,#20043,#20044,#20045,#20046,#20047,#20048,#20049,
#20050,#20051,#20052,#20053,#20054,#20055,#20056,#20057,#20058,#20059,#20060),
 .UNSPECIFIED.,.F.,.F.,(4,3,3,3,3,3,3,3,3,3,3,3,3,3,3,3,3,3,3,3,3,3,3,3,
3,3,3,4),(0.,0.0295773881143737,0.0605304169685423,0.0926266479893201,0.126171922797343,
0.161663359409954,0.200029752325282,0.243548698800364,0.310961877359763,
0.354026760024778,0.394400087523229,0.429679984526457,0.462839399613297,
0.494661354046568,0.527132669669348,0.560640871664874,0.596011154103228,
0.63407950774038,0.676959315395981,0.757719486546985,0.799022960216542,
0.836244253898911,0.871055469579005,0.90343521020651,0.934833075276548,
0.965406057021946,0.995023142066622,1.),.UNSPECIFIED.);
#128=B_SPLINE_CURVE_WITH_KNOTS('',3,(#20087,#20088,#20089,#20090,#20091,
#20092),.UNSPECIFIED.,.F.,.F.,(4,2,4),(9.99629094513175E-5,0.155241085196768,
0.273153287835103),.UNSPECIFIED.);
#129=B_SPLINE_CURVE_WITH_KNOTS('',3,(#20095,#20096,#20097,#20098,#20099,
#20100),.UNSPECIFIED.,.F.,.F.,(4,2,4),(-0.273153287835103,-0.155241085196768,
-9.99629094513175E-5),.UNSPECIFIED.);
#130=B_SPLINE_CURVE_WITH_KNOTS('',3,(#20126,#20127,#20128,#20129),
 .UNSPECIFIED.,.F.,.F.,(4,4),(-0.310482170393535,-0.273153287835089),
 .UNSPECIFIED.);
#131=B_SPLINE_CURVE_WITH_KNOTS('',3,(#20130,#20131,#20132,#20133),
 .UNSPECIFIED.,.F.,.F.,(4,4),(0.273153287835089,0.310482170393535),
 .UNSPECIFIED.);
#132=B_SPLINE_CURVE_WITH_KNOTS('',3,(#20159,#20160,#20161,#20162,#20163,
#20164),.UNSPECIFIED.,.F.,.F.,(4,2,4),(-0.945184496035905,-0.778344160365423,
-0.67569543130222),.UNSPECIFIED.);
#133=B_SPLINE_CURVE_WITH_KNOTS('',3,(#20167,#20168,#20169,#20170,#20171,
#20172),.UNSPECIFIED.,.F.,.F.,(4,2,4),(0.67569543130222,0.778344160365423,
0.945184496035905),.UNSPECIFIED.);
#134=B_SPLINE_CURVE_WITH_KNOTS('',3,(#20189,#20190,#20191,#20192),
 .UNSPECIFIED.,.F.,.F.,(4,4),(-0.675695431302257,-0.639351607098027),
 .UNSPECIFIED.);
#135=B_SPLINE_CURVE_WITH_KNOTS('',3,(#20193,#20194,#20195,#20196),
 .UNSPECIFIED.,.F.,.F.,(4,4),(0.639351607098027,0.675695431302257),
 .UNSPECIFIED.);
#136=B_SPLINE_CURVE_WITH_KNOTS('',3,(#20199,#20200,#20201,#20202,#20203,
#20204,#20205,#20206,#20207,#20208,#20209,#20210,#20211,#20212,#20213,#20214,
#20215,#20216,#20217,#20218,#20219,#20220,#20221,#20222,#20223,#20224,#20225,
#20226,#20227,#20228,#20229,#20230,#20231,#20232,#20233,#20234,#20235,#20236,
#20237,#20238,#20239,#20240,#20241,#20242,#20243,#20244,#20245,#20246,#20247,
#20248,#20249,#20250,#20251,#20252,#20253,#20254,#20255,#20256,#20257,#20258,
#20259,#20260,#20261,#20262,#20263,#20264,#20265,#20266,#20267,#20268,#20269,
#20270,#20271,#20272,#20273,#20274,#20275,#20276,#20277,#20278,#20279,#20280),
 .UNSPECIFIED.,.F.,.F.,(4,3,3,3,3,3,3,3,3,3,3,3,3,3,3,3,3,3,3,3,3,3,3,3,
3,3,3,4),(0.,0.0295774172384458,0.0605304778777659,0.0926267436200908,0.126172057442769,
0.161663540018093,0.200029992233166,0.243549050668545,0.310961698223174,
0.354026592084225,0.394399930078961,0.429679866520511,0.462839301683719,
0.494661290298148,0.527132633260964,0.560640855188699,0.596011159218635,
0.634079537198202,0.676959378678976,0.757719534009232,0.799023032825097,
0.836244348173232,0.871055583738876,0.90343534360451,0.934833227096761,
0.965406226610612,0.9950233300335,1.),.UNSPECIFIED.);
#137=B_SPLINE_CURVE_WITH_KNOTS('',3,(#20282,#20283,#20284,#20285,#20286,
#20287),.UNSPECIFIED.,.F.,.F.,(4,2,4),(-0.269588855200419,-0.166940126137213,
-9.97881403247492E-5),.UNSPECIFIED.);
#138=B_SPLINE_CURVE_WITH_KNOTS('',3,(#20313,#20314,#20315,#20316,#20317,
#20318,#20319,#20320,#20321,#20322,#20323,#20324,#20325,#20326,#20327,#20328,
#20329,#20330,#20331,#20332,#20333,#20334,#20335,#20336,#20337,#20338,#20339,
#20340,#20341,#20342,#20343,#20344,#20345,#20346,#20347,#20348,#20349,#20350,
#20351,#20352,#20353,#20354,#20355,#20356,#20357,#20358,#20359,#20360,#20361,
#20362,#20363,#20364,#20365,#20366,#20367,#20368,#20369,#20370,#20371,#20372,
#20373,#20374,#20375,#20376,#20377,#20378,#20379,#20380,#20381,#20382,#20383,
#20384,#20385,#20386,#20387,#20388,#20389,#20390,#20391,#20392,#20393,#20394),
 .UNSPECIFIED.,.F.,.F.,(4,3,3,3,3,3,3,3,3,3,3,3,3,3,3,3,3,3,3,3,3,3,3,3,
3,3,3,4),(0.,0.0295705059225161,0.060515948666961,0.0926038162606335,0.126139587093134,
0.161619668950802,0.199971107042965,0.243460414554639,0.310976439007705,
0.354040411569723,0.394412885846616,0.429686039982354,0.462833624458519,
0.494651028937031,0.527129557030648,0.560643519234301,0.596019929713648,
0.634095033602234,0.676984117122705,0.757738087842029,0.799051738229506,
0.836280906721543,0.871099048168231,0.903485294448113,0.934889313350476,
0.96546817471544,0.995091328163233,1.),.UNSPECIFIED.);
#139=B_SPLINE_CURVE_WITH_KNOTS('',3,(#20395,#20396,#20397,#20398),
 .UNSPECIFIED.,.F.,.F.,(4,4),(-1.,0.),.UNSPECIFIED.);
#140=B_SPLINE_CURVE_WITH_KNOTS('',3,(#20436,#20437,#20438,#20439),
 .UNSPECIFIED.,.F.,.F.,(4,4),(0.,1.),.UNSPECIFIED.);
#141=B_SPLINE_CURVE_WITH_KNOTS('',3,(#20487,#20488,#20489,#20490),
 .UNSPECIFIED.,.F.,.F.,(4,4),(-0.305932679404608,-0.269588855200382),
 .UNSPECIFIED.);
#142=B_SPLINE_CURVE_WITH_KNOTS('',3,(#20516,#20517,#20518,#20519,#20520,
#20521),.UNSPECIFIED.,.F.,.F.,(4,2,4),(-0.954283455385462,-0.79914218328373,
-0.681229980645395),.UNSPECIFIED.);
#143=B_SPLINE_CURVE_WITH_KNOTS('',3,(#20539,#20540,#20541,#20542),
 .UNSPECIFIED.,.F.,.F.,(4,4),(-0.681229980645409,-0.643901098086962),
 .UNSPECIFIED.);
#144=B_SPLINE_CURVE_WITH_KNOTS('',3,(#20556,#20557,#20558,#20559,#20560,
#20561),.UNSPECIFIED.,.F.,.F.,(4,2,4),(0.,0.155241085196768,0.310482170393537),
 .UNSPECIFIED.);
#145=B_SPLINE_CURVE_WITH_KNOTS('',3,(#20565,#20566,#20567,#20568,#20569,
#20570),.UNSPECIFIED.,.F.,.F.,(4,2,4),(0.643901098086962,0.79914218328373,
0.954383268480499),.UNSPECIFIED.);
#146=B_SPLINE_CURVE_WITH_KNOTS('',3,(#20572,#20573,#20574,#20575,#20576,
#20577),.UNSPECIFIED.,.F.,.F.,(4,2,4),(0.,0.15524108519677,0.31048217039354),
 .UNSPECIFIED.);
#147=B_SPLINE_CURVE_WITH_KNOTS('',3,(#20580,#20581,#20582,#20583,#20584,
#20585),.UNSPECIFIED.,.F.,.F.,(4,2,4),(0.643901098086964,0.799142183283734,
0.954383268480504),.UNSPECIFIED.);
#148=B_SPLINE_CURVE_WITH_KNOTS('',3,(#20591,#20592,#20593,#20594,#20595,
#20596),.UNSPECIFIED.,.F.,.F.,(4,2,4),(0.,0.155241085196768,0.310482170393535),
 .UNSPECIFIED.);
#149=B_SPLINE_CURVE_WITH_KNOTS('',3,(#20601,#20602,#20603,#20604,#20605,
#20606),.UNSPECIFIED.,.F.,.F.,(4,2,4),(0.643901098086961,0.799142183283728,
0.954383268480496),.UNSPECIFIED.);
#150=B_SPLINE_CURVE_WITH_KNOTS('',3,(#20608,#20609,#20610,#20611,#20612,
#20613),.UNSPECIFIED.,.F.,.F.,(4,2,4),(0.,0.166940126137215,0.305932679404607),
 .UNSPECIFIED.);
#151=B_SPLINE_CURVE_WITH_KNOTS('',3,(#20616,#20617,#20618,#20619,#20620,
#20621),.UNSPECIFIED.,.F.,.F.,(4,2,4),(0.643908930969365,0.799150016166133,
0.954391101362901),.UNSPECIFIED.);
#152=B_SPLINE_CURVE_WITH_KNOTS('',3,(#20657,#20658,#20659,#20660,#20661,
#20662,#20663,#20664,#20665,#20666,#20667,#20668,#20669,#20670,#20671,#20672,
#20673,#20674,#20675,#20676,#20677,#20678,#20679,#20680,#20681,#20682,#20683,
#20684,#20685,#20686,#20687,#20688,#20689,#20690,#20691,#20692,#20693,#20694,
#20695,#20696,#20697,#20698,#20699,#20700,#20701,#20702),.UNSPECIFIED.,
 .F.,.F.,(4,3,3,3,3,3,3,3,3,3,3,3,3,3,3,4),(0.,0.0572017311997787,0.120330894890366,
0.190833525217158,0.280000607595836,0.370000531646356,0.437396979142466,
0.498588004587218,0.56260087810271,0.634065239675333,0.727489847564673,
0.803842080660462,0.870326860442866,0.931777978459012,0.988871097354878,
1.),.UNSPECIFIED.);
#153=B_SPLINE_CURVE_WITH_KNOTS('',3,(#20704,#20705,#20706,#20707),
 .UNSPECIFIED.,.F.,.F.,(4,4),(0.,1.),.UNSPECIFIED.);
#154=B_SPLINE_CURVE_WITH_KNOTS('',3,(#20709,#20710,#20711,#20712,#20713,
#20714,#20715,#20716,#20717,#20718,#20719,#20720,#20721,#20722,#20723,#20724,
#20725,#20726,#20727,#20728,#20729,#20730,#20731,#20732,#20733,#20734,#20735,
#20736,#20737,#20738,#20739,#20740,#20741,#20742,#20743,#20744,#20745,#20746,
#20747,#20748,#20749,#20750,#20751,#20752,#20753,#20754),.UNSPECIFIED.,
 .F.,.F.,(4,3,3,3,3,3,3,3,3,3,3,3,3,3,3,4),(0.,0.0572030252319241,0.12033380234495,
0.190838689074404,0.28001183745251,0.370010357770946,0.43740667017455,0.498598114868611,
0.562610573399873,0.634075370124963,0.727505599815991,0.803852814389783,
0.870334971805663,0.931784146691265,0.988875797348581,1.),.UNSPECIFIED.);
#155=B_SPLINE_CURVE_WITH_KNOTS('',3,(#20782,#20783,#20784,#20785,#20786,
#20787,#20788,#20789,#20790,#20791,#20792,#20793,#20794,#20795,#20796,#20797,
#20798,#20799,#20800,#20801,#20802,#20803,#20804,#20805,#20806,#20807,#20808,
#20809,#20810,#20811,#20812,#20813,#20814,#20815,#20816,#20817,#20818,#20819,
#20820,#20821,#20822,#20823,#20824,#20825,#20826,#20827),.UNSPECIFIED.,
 .F.,.F.,(4,3,3,3,3,3,3,3,3,3,3,3,3,3,3,4),(0.,0.0572017311995356,0.120330894891212,
0.190833525222983,0.280000607602918,0.370000531652553,0.437396979149437,
0.498588004587769,0.562600878102254,0.634065239673979,0.727489847577867,
0.803842080671477,0.870326860452954,0.931777978465078,0.988871097360322,
1.),.UNSPECIFIED.);
#156=B_SPLINE_CURVE_WITH_KNOTS('',3,(#20829,#20830,#20831,#20832),
 .UNSPECIFIED.,.F.,.F.,(4,4),(0.,1.),.UNSPECIFIED.);
#157=B_SPLINE_CURVE_WITH_KNOTS('',3,(#20834,#20835,#20836,#20837,#20838,
#20839,#20840,#20841,#20842,#20843,#20844,#20845,#20846,#20847,#20848,#20849,
#20850,#20851,#20852,#20853,#20854,#20855,#20856,#20857,#20858,#20859,#20860,
#20861,#20862,#20863,#20864,#20865,#20866,#20867,#20868,#20869,#20870,#20871,
#20872,#20873,#20874,#20875,#20876,#20877,#20878,#20879),.UNSPECIFIED.,
 .F.,.F.,(4,3,3,3,3,3,3,3,3,3,3,3,3,3,3,4),(0.,0.0572030252292159,0.120333802342511,
0.190838689073324,0.280011837455233,0.370010357773329,0.437406670176794,
0.498598114483872,0.562610572991308,0.634075369653291,0.72750559895434,
0.803852813688791,0.870334971170512,0.931784146099022,0.988875796770373,
1.),.UNSPECIFIED.);
#158=B_SPLINE_CURVE_WITH_KNOTS('',3,(#20910,#20911,#20912,#20913,#20914,
#20915,#20916),.UNSPECIFIED.,.F.,.F.,(4,1,1,1,4),(-1.70953476876621,-1.22109626340444,
-0.732657758042664,-0.366328879021332,5.55111512312578E-17),
 .UNSPECIFIED.);
#159=B_SPLINE_CURVE_WITH_KNOTS('',3,(#20919,#20920,#20921,#20922,#20923,
#20924,#20925),.UNSPECIFIED.,.F.,.F.,(4,1,1,1,4),(-5.55111512312578E-17,
0.366328879021332,0.732657758042664,1.22109626340444,1.70953476876621),
 .UNSPECIFIED.);
#160=B_SPLINE_CURVE_WITH_KNOTS('',3,(#20956,#20957,#20958,#20959,#20960,
#20961),.UNSPECIFIED.,.F.,.F.,(4,1,1,4),(-1.70953476876627,-0.976877010723583,
-0.488438505361791,0.),.UNSPECIFIED.);
#161=B_SPLINE_CURVE_WITH_KNOTS('',3,(#20962,#20963,#20964,#20965,#20966,
#20967),.UNSPECIFIED.,.F.,.F.,(4,1,1,4),(0.,0.488438505361791,0.976877010723583,
1.70953476876627),.UNSPECIFIED.);
#162=B_SPLINE_CURVE_WITH_KNOTS('',3,(#20972,#20973,#20974,#20975,#20976,
#20977),.UNSPECIFIED.,.F.,.F.,(4,1,1,4),(-1.70953476876625,-0.976877010723563,
-0.48843850536177,2.22044604925036E-14),.UNSPECIFIED.);
#163=B_SPLINE_CURVE_WITH_KNOTS('',3,(#20979,#20980,#20981,#20982,#20983,
#20984,#20985,#20986,#20987,#20988,#20989,#20990,#20991,#20992,#20993,#20994,
#20995,#20996,#20997,#20998,#20999,#21000,#21001,#21002,#21003,#21004,#21005,
#21006,#21007,#21008,#21009,#21010,#21011,#21012,#21013,#21014,#21015,#21016,
#21017,#21018,#21019,#21020,#21021,#21022,#21023,#21024),.UNSPECIFIED.,
 .F.,.F.,(4,3,3,3,3,3,3,3,3,3,3,3,3,3,3,4),(0.,0.0572017312010985,0.120330894892007,
0.190833525228125,0.28000060761627,0.370000531664237,0.437396979166382,
0.498588004436113,0.562600877944707,0.634065239485818,0.727489847210369,
0.803842080370144,0.870326860183826,0.931777978218593,0.988871097121157,
1.),.UNSPECIFIED.);
#164=B_SPLINE_CURVE_WITH_KNOTS('',3,(#21034,#21035,#21036,#21037,#21038,
#21039,#21040,#21041,#21042,#21043,#21044,#21045,#21046,#21047,#21048,#21049,
#21050,#21051,#21052,#21053,#21054,#21055,#21056,#21057,#21058,#21059,#21060,
#21061,#21062,#21063,#21064,#21065,#21066,#21067,#21068,#21069,#21070,#21071,
#21072,#21073,#21074,#21075,#21076,#21077,#21078,#21079),.UNSPECIFIED.,
 .F.,.F.,(4,3,3,3,3,3,3,3,3,3,3,3,3,3,3,4),(0.,0.0572030252297135,0.120333802345235,
0.19083868907026,0.280011837447865,0.370010357766881,0.437406670170065,
0.498598115100775,0.562610573648761,0.634075370412809,0.727505600383724,
0.803852814849948,0.870334972221295,0.931784147083444,0.988875797723589,
1.),.UNSPECIFIED.);
#165=B_SPLINE_CURVE_WITH_KNOTS('',3,(#21080,#21081,#21082,#21083,#21084,
#21085),.UNSPECIFIED.,.F.,.F.,(4,1,1,4),(-2.2204460492503E-14,0.488438505361761,
0.976877010723545,1.70953476876622),.UNSPECIFIED.);
#166=B_SPLINE_CURVE_WITH_KNOTS('',3,(#21123,#21124,#21125,#21126),
 .UNSPECIFIED.,.F.,.F.,(4,4),(0.,1.),.UNSPECIFIED.);
#167=B_SPLINE_CURVE_WITH_KNOTS('',3,(#21128,#21129,#21130,#21131,#21132,
#21133,#21134,#21135,#21136,#21137,#21138,#21139,#21140,#21141,#21142,#21143,
#21144,#21145,#21146,#21147,#21148,#21149,#21150,#21151,#21152,#21153,#21154,
#21155,#21156,#21157,#21158,#21159,#21160,#21161,#21162,#21163,#21164,#21165,
#21166,#21167,#21168,#21169,#21170,#21171,#21172,#21173),.UNSPECIFIED.,
 .F.,.F.,(4,3,3,3,3,3,3,3,3,3,3,3,3,3,3,4),(0.,0.0572030252310299,0.120333802344518,
0.190838689075309,0.280011837457742,0.370010357775524,0.437406670179767,
0.498598114793286,0.562610573319674,0.634075370032691,0.727505599642952,
0.803852814249658,0.870334971678365,0.931784146571623,0.988875797229984,
1.),.UNSPECIFIED.);
#168=B_SPLINE_CURVE_WITH_KNOTS('',3,(#21200,#21201,#21202,#21203,#21204,
#21205,#21206,#21207,#21208,#21209,#21210,#21211,#21212,#21213,#21214,#21215,
#21216,#21217,#21218,#21219,#21220,#21221,#21222,#21223,#21224,#21225,#21226,
#21227,#21228,#21229,#21230,#21231,#21232,#21233,#21234,#21235,#21236,#21237,
#21238,#21239,#21240,#21241,#21242,#21243,#21244,#21245),.UNSPECIFIED.,
 .F.,.F.,(4,3,3,3,3,3,3,3,3,3,3,3,3,3,3,4),(0.,0.0572017311978579,0.120330894888584,
0.190833525218063,0.280000607593651,0.370000531644445,0.437396979144834,
0.498588004278573,0.562600877772937,0.634065239292226,0.727489846889499,
0.803842080110613,0.87032685994332,0.931777977987771,0.988871096896156,
1.),.UNSPECIFIED.);
#169=B_SPLINE_CURVE_WITH_KNOTS('',3,(#21246,#21247,#21248,#21249),
 .UNSPECIFIED.,.F.,.F.,(4,4),(0.,1.),.UNSPECIFIED.);
#170=B_SPLINE_CURVE_WITH_KNOTS('',3,(#21275,#21276,#21277,#21278,#21279,
#21280),.UNSPECIFIED.,.F.,.F.,(4,1,1,4),(-1.70953476876622,-0.976877010723545,
-0.488438505361761,2.2204460492503E-14),.UNSPECIFIED.);
#171=B_SPLINE_CURVE_WITH_KNOTS('',3,(#21310,#21311,#21312,#21313,#21314,
#21315),.UNSPECIFIED.,.F.,.F.,(4,1,1,4),(-2.22044604925036E-14,0.48843850536177,
0.976877010723563,1.70953476876625),.UNSPECIFIED.);
#172=B_SPLINE_CURVE_WITH_KNOTS('',3,(#21320,#21321,#21322,#21323,#21324,
#21325),.UNSPECIFIED.,.F.,.F.,(4,1,1,4),(-1.70953476876624,-0.976877010723568,
-0.488438505361784,0.),.UNSPECIFIED.);
#173=B_SPLINE_CURVE_WITH_KNOTS('',3,(#21327,#21328,#21329,#21330,#21331,
#21332,#21333,#21334,#21335,#21336,#21337,#21338,#21339,#21340,#21341,#21342,
#21343,#21344,#21345,#21346,#21347,#21348,#21349,#21350,#21351,#21352,#21353,
#21354,#21355,#21356,#21357,#21358,#21359,#21360,#21361,#21362,#21363,#21364,
#21365,#21366,#21367,#21368,#21369,#21370,#21371,#21372),.UNSPECIFIED.,
 .F.,.F.,(4,3,3,3,3,3,3,3,3,3,3,3,3,3,3,4),(0.,0.0572017312023357,0.120330894894396,
0.190833525223119,0.280000607603027,0.370000531652649,0.437396979148621,
0.498588004437818,0.562600877943201,0.634065239490927,0.727489847224149,
0.803842080384343,0.870326860191725,0.931777978222192,0.988871097126222,
1.),.UNSPECIFIED.);
#174=B_SPLINE_CURVE_WITH_KNOTS('',3,(#21380,#21381,#21382,#21383,#21384,
#21385,#21386,#21387,#21388,#21389,#21390,#21391,#21392,#21393,#21394,#21395,
#21396,#21397,#21398,#21399,#21400,#21401,#21402,#21403,#21404,#21405,#21406,
#21407,#21408,#21409,#21410,#21411,#21412,#21413,#21414,#21415,#21416,#21417,
#21418,#21419,#21420,#21421,#21422,#21423,#21424,#21425),.UNSPECIFIED.,
 .F.,.F.,(4,3,3,3,3,3,3,3,3,3,3,3,3,3,3,4),(0.,0.0572030252293332,0.120333802342866,
0.190838689071281,0.280011837454217,0.37001035777244,0.437406670175742,
0.498598114943859,0.562610573478433,0.634075370216571,0.727505599976586,
0.803852814520644,0.870334971919668,0.93178414679375,0.988875797446903,
1.),.UNSPECIFIED.);
#175=B_SPLINE_CURVE_WITH_KNOTS('',3,(#21426,#21427,#21428,#21429,#21430,
#21431),.UNSPECIFIED.,.F.,.F.,(4,1,1,4),(0.,0.488438505361779,0.976877010723558,
1.70953476876623),.UNSPECIFIED.);
#176=B_SPLINE_CURVE_WITH_KNOTS('',3,(#21457,#21458,#21459,#21460,#21461,
#21462,#21463,#21464,#21465,#21466,#21467,#21468,#21469,#21470,#21471,#21472,
#21473,#21474,#21475,#21476,#21477,#21478,#21479,#21480,#21481,#21482,#21483,
#21484,#21485,#21486,#21487,#21488,#21489,#21490,#21491,#21492,#21493,#21494,
#21495,#21496,#21497,#21498,#21499,#21500,#21501,#21502),.UNSPECIFIED.,
 .F.,.F.,(4,3,3,3,3,3,3,3,3,3,3,3,3,3,3,4),(0.,0.0572017311998059,0.120330894890615,
0.190833525219348,0.280000607590358,0.370000531641563,0.437396979142138,
0.498588004431166,0.562600877935177,0.634065239482274,0.72748984722562,
0.803842080384528,0.870326860191735,0.931777978221736,0.988871097122214,
1.),.UNSPECIFIED.);
#177=B_SPLINE_CURVE_WITH_KNOTS('',3,(#21503,#21504,#21505,#21506),
 .UNSPECIFIED.,.F.,.F.,(4,4),(0.,1.),.UNSPECIFIED.);
#178=B_SPLINE_CURVE_WITH_KNOTS('',3,(#21532,#21533,#21534,#21535),
 .UNSPECIFIED.,.F.,.F.,(4,4),(0.,1.),.UNSPECIFIED.);
#179=B_SPLINE_CURVE_WITH_KNOTS('',3,(#21537,#21538,#21539,#21540,#21541,
#21542,#21543,#21544,#21545,#21546,#21547,#21548,#21549,#21550,#21551,#21552,
#21553,#21554,#21555,#21556,#21557,#21558,#21559,#21560,#21561,#21562,#21563,
#21564,#21565,#21566,#21567,#21568,#21569,#21570,#21571,#21572,#21573,#21574,
#21575,#21576,#21577,#21578,#21579,#21580,#21581,#21582),.UNSPECIFIED.,
 .F.,.F.,(4,3,3,3,3,3,3,3,3,3,3,3,3,3,3,4),(0.,0.0572030252325847,0.120333802345704,
0.190838689075859,0.280011837455415,0.370010357773488,0.437406670178867,
0.498598114640677,0.562610573158014,0.634075369846179,0.727505599307959,
0.803852813976729,0.870334971429114,0.931784146336173,0.98887579700217,
1.),.UNSPECIFIED.);
#180=B_SPLINE_CURVE_WITH_KNOTS('',3,(#21610,#21611,#21612,#21613,#21614,
#21615),.UNSPECIFIED.,.F.,.F.,(4,1,1,4),(0.,0.488438505361784,0.976877010723568,
1.70953476876624),.UNSPECIFIED.);
#181=B_SPLINE_CURVE_WITH_KNOTS('',3,(#21644,#21645,#21646,#21647,#21648,
#21649),.UNSPECIFIED.,.F.,.F.,(4,1,1,4),(-1.70953476876623,-0.976877010723558,
-0.488438505361779,0.),.UNSPECIFIED.);
#182=B_SPLINE_CURVE_WITH_KNOTS('',3,(#21675,#21676,#21677,#21678,#21679,
#21680,#21681,#21682,#21683,#21684,#21685,#21686,#21687,#21688,#21689,#21690,
#21691,#21692,#21693,#21694,#21695,#21696,#21697,#21698,#21699,#21700,#21701,
#21702,#21703,#21704,#21705,#21706,#21707,#21708,#21709,#21710,#21711,#21712,
#21713,#21714,#21715,#21716,#21717,#21718,#21719,#21720),.UNSPECIFIED.,
 .F.,.F.,(4,3,3,3,3,3,3,3,3,3,3,3,3,3,3,4),(0.,0.0572017311990066,0.12033089488981,
0.190833525218569,0.280000607592288,0.370000531643252,0.437396979144409,
0.498588004504094,0.562600878013463,0.634065239570545,0.727489847383163,
0.803842080513076,0.87032686030984,0.931777978330153,0.988871097227407,
1.),.UNSPECIFIED.);
#183=B_SPLINE_CURVE_WITH_KNOTS('',3,(#21722,#21723,#21724,#21725),
 .UNSPECIFIED.,.F.,.F.,(4,4),(-1.,0.),.UNSPECIFIED.);
#184=B_SPLINE_CURVE_WITH_KNOTS('',3,(#21726,#21727,#21728,#21729,#21730,
#21731,#21732,#21733,#21734,#21735,#21736,#21737,#21738,#21739,#21740,#21741,
#21742,#21743,#21744,#21745,#21746,#21747,#21748,#21749,#21750,#21751,#21752,
#21753,#21754,#21755,#21756,#21757,#21758,#21759,#21760,#21761,#21762,#21763,
#21764,#21765,#21766,#21767,#21768,#21769,#21770,#21771),.UNSPECIFIED.,
 .F.,.F.,(4,3,3,3,3,3,3,3,3,3,3,3,3,3,3,4),(0.,0.0572030252278138,0.120333802343175,
0.190838689074842,0.280011837442225,0.370010357761947,0.437406670170392,
0.498598115021839,0.562610573562917,0.634075370316736,0.727505600127926,
0.803852814646169,0.87033497203609,0.931784146912104,0.988875797559871,
1.),.UNSPECIFIED.);
#185=B_SPLINE_CURVE_WITH_KNOTS('',3,(#21798,#21799,#21800,#21801,#21802,
#21803,#21804,#21805,#21806,#21807,#21808,#21809,#21810,#21811,#21812,#21813,
#21814,#21815,#21816,#21817,#21818,#21819,#21820,#21821,#21822,#21823,#21824,
#21825,#21826,#21827,#21828,#21829,#21830,#21831,#21832,#21833,#21834,#21835,
#21836,#21837,#21838,#21839,#21840,#21841,#21842,#21843),.UNSPECIFIED.,
 .F.,.F.,(4,3,3,3,3,3,3,3,3,3,3,3,3,3,3,4),(0.,0.0572017312051678,0.12033089489696,
0.190833525228863,0.280000607608025,0.370000531657022,0.437396979162787,
0.498588004452882,0.562600877959885,0.63406523951468,0.727489847284879,
0.803842080435825,0.870326860243776,0.93177797826367,0.988871097172671,
1.),.UNSPECIFIED.);
#186=B_SPLINE_CURVE_WITH_KNOTS('',3,(#21845,#21846,#21847,#21848),
 .UNSPECIFIED.,.F.,.F.,(4,4),(0.,1.),.UNSPECIFIED.);
#187=B_SPLINE_CURVE_WITH_KNOTS('',3,(#21850,#21851,#21852,#21853,#21854,
#21855,#21856,#21857,#21858,#21859,#21860,#21861,#21862,#21863,#21864,#21865,
#21866,#21867,#21868,#21869,#21870,#21871,#21872,#21873,#21874,#21875,#21876,
#21877,#21878,#21879,#21880,#21881,#21882,#21883,#21884,#21885,#21886,#21887,
#21888,#21889,#21890,#21891,#21892,#21893,#21894,#21895),.UNSPECIFIED.,
 .F.,.F.,(4,3,3,3,3,3,3,3,3,3,3,3,3,3,3,4),(0.,0.0572030252315006,0.120333802344992,
0.190838689075267,0.280011837456553,0.370010357774484,0.437406670177093,
0.498598114715166,0.562610573236497,0.634075369937252,0.727505599475578,
0.803852814112987,0.870334971553103,0.931784146452336,0.988875797114711,
1.),.UNSPECIFIED.);
#188=B_SPLINE_CURVE_WITH_KNOTS('',3,(#21922,#21923,#21924,#21925,#21926,
#21927),.UNSPECIFIED.,.F.,.F.,(4,1,1,4),(-1.7095347687662,-0.97687701072354,
-0.488438505361764,1.11854969730985E-14),.UNSPECIFIED.);
#189=B_SPLINE_CURVE_WITH_KNOTS('',3,(#21930,#21931,#21932,#21933,#21934,
#21935),.UNSPECIFIED.,.F.,.F.,(4,1,1,4),(-1.11854969730985E-14,0.488438505361764,
0.97687701072354,1.7095347687662),.UNSPECIFIED.);
#190=B_SPLINE_CURVE_WITH_KNOTS('',3,(#21966,#21967,#21968,#21969,#21970,
#21971),.UNSPECIFIED.,.F.,.F.,(4,1,1,4),(1.43205788482356,2.16471564286623,
2.65315414822802,3.1415926535898),.UNSPECIFIED.);
#191=B_SPLINE_CURVE_WITH_KNOTS('',3,(#21972,#21973,#21974,#21975,#21976,
#21977),.UNSPECIFIED.,.F.,.F.,(4,1,1,4),(-3.1415926535898,-2.65315414822802,
-2.16471564286623,-1.43205788482356),.UNSPECIFIED.);
#192=B_SPLINE_CURVE_WITH_KNOTS('',3,(#22664,#22665,#22666,#22667,#22668,
#22669,#22670,#22671,#22672,#22673,#22674,#22675,#22676,#22677,#22678,#22679,
#22680,#22681,#22682,#22683,#22684,#22685,#22686,#22687,#22688,#22689,#22690,
#22691,#22692,#22693,#22694,#22695,#22696,#22697,#22698,#22699,#22700,#22701,
#22702,#22703,#22704,#22705,#22706,#22707,#22708,#22709,#22710,#22711,#22712,
#22713,#22714,#22715,#22716,#22717,#22718,#22719,#22720,#22721,#22722,#22723,
#22724,#22725,#22726,#22727,#22728,#22729,#22730,#22731,#22732,#22733,#22734,
#22735,#22736,#22737,#22738,#22739,#22740,#22741,#22742,#22743,#22744,#22745),
 .UNSPECIFIED.,.F.,.F.,(4,3,3,3,3,3,3,3,3,3,3,3,3,3,3,3,3,3,3,3,3,3,3,3,
3,3,3,4),(0.,0.0295705059221788,0.060515948666938,0.0926038162611793,0.126139587094163,
0.161619668951817,0.19997110704497,0.243460414557959,0.310976439008441,
0.354040411570413,0.394412885847263,0.429686039983613,0.462833624459996,
0.494651028940637,0.527129557033639,0.560643519237532,0.596019929716605,
0.634095033607031,0.676984117127751,0.757738087845813,0.799051738230702,
0.836280906722732,0.871099048170047,0.903485294449899,0.934889313351429,
0.965468174714213,0.9950913281628,1.),.UNSPECIFIED.);
#193=B_SPLINE_CURVE_WITH_KNOTS('',3,(#22747,#22748,#22749,#22750),
 .UNSPECIFIED.,.F.,.F.,(4,4),(-1.,0.),.UNSPECIFIED.);
#194=B_SPLINE_CURVE_WITH_KNOTS('',3,(#22752,#22753,#22754,#22755,#22756,
#22757,#22758,#22759,#22760,#22761,#22762,#22763,#22764,#22765,#22766,#22767,
#22768,#22769,#22770,#22771,#22772,#22773,#22774,#22775,#22776,#22777,#22778,
#22779,#22780,#22781,#22782,#22783,#22784,#22785,#22786,#22787,#22788,#22789,
#22790,#22791,#22792,#22793,#22794,#22795,#22796,#22797,#22798,#22799,#22800,
#22801,#22802,#22803),.UNSPECIFIED.,.F.,.F.,(4,3,3,3,3,3,3,3,3,3,3,3,3,
3,3,3,3,4),(0.,0.0499444622912523,0.102213229602865,0.161337747228745,0.226027789144595,
0.322774315501521,0.388018395848048,0.444871194111793,0.498045969161039,
0.55130803854745,0.608971254047864,0.676370635210691,0.757277976408018,
0.819640075218638,0.876287936111095,0.929442920609184,0.979183148027167,
1.),.UNSPECIFIED.);
#195=B_SPLINE_CURVE_WITH_KNOTS('',3,(#22843,#22844,#22845,#22846,#22847,
#22848,#22849,#22850,#22851,#22852,#22853,#22854,#22855,#22856,#22857,#22858,
#22859,#22860,#22861,#22862,#22863,#22864,#22865,#22866,#22867,#22868,#22869,
#22870,#22871,#22872,#22873,#22874,#22875,#22876,#22877,#22878,#22879,#22880,
#22881,#22882,#22883,#22884,#22885,#22886,#22887,#22888,#22889,#22890,#22891,
#22892,#22893,#22894),.UNSPECIFIED.,.F.,.F.,(4,3,3,3,3,3,3,3,3,3,3,3,3,
3,3,3,3,4),(0.,0.0499441826810774,0.102212661913948,0.161336812389012,0.22602629684231,
0.322773009737021,0.388016976561433,0.444869601982627,0.498043895325567,
0.551305755159732,0.608968423870093,0.676366592453384,0.757274944340038,
0.819637084908965,0.876284880238144,0.929439762109144,0.979179823244059,
1.),.UNSPECIFIED.);
#196=B_SPLINE_CURVE_WITH_KNOTS('',3,(#22896,#22897,#22898,#22899),
 .UNSPECIFIED.,.F.,.F.,(4,4),(0.,1.),.UNSPECIFIED.);
#197=B_SPLINE_CURVE_WITH_KNOTS('',3,(#22901,#22902,#22903,#22904,#22905,
#22906,#22907,#22908,#22909,#22910,#22911,#22912,#22913,#22914,#22915,#22916,
#22917,#22918,#22919,#22920,#22921,#22922,#22923,#22924,#22925,#22926,#22927,
#22928,#22929,#22930,#22931,#22932,#22933,#22934,#22935,#22936,#22937,#22938,
#22939,#22940,#22941,#22942,#22943,#22944,#22945,#22946,#22947,#22948,#22949,
#22950,#22951,#22952,#22953,#22954,#22955,#22956,#22957,#22958,#22959,#22960,
#22961,#22962,#22963,#22964,#22965,#22966,#22967,#22968,#22969,#22970,#22971,
#22972,#22973,#22974,#22975,#22976,#22977,#22978,#22979,#22980,#22981,#22982),
 .UNSPECIFIED.,.F.,.F.,(4,3,3,3,3,3,3,3,3,3,3,3,3,3,3,3,3,3,3,3,3,3,3,3,
3,3,3,4),(0.,0.0295773881145616,0.060530416968692,0.0926266479896254,0.126171922797507,
0.161663359409179,0.200029752326511,0.243548698803929,0.310961877352299,
0.35402676001778,0.394400087516669,0.429679984519188,0.462839399605369,
0.494661354038637,0.527132669662275,0.560640871657354,0.59601115409547,
0.63407950773062,0.676959315385358,0.757719486539019,0.799022960212248,
0.836244253893979,0.871055469575998,0.903435210203506,0.934833075272902,
0.965406057017476,0.995023142061764,1.),.UNSPECIFIED.);
#198=B_SPLINE_CURVE_WITH_KNOTS('',3,(#23001,#23002,#23003,#23004),
 .UNSPECIFIED.,.F.,.F.,(4,4),(9.99629094513139E-5,0.273153287835102),
 .UNSPECIFIED.);
#199=B_SPLINE_CURVE_WITH_KNOTS('',3,(#23007,#23008,#23009,#23010),
 .UNSPECIFIED.,.F.,.F.,(4,4),(-0.273153287835102,-9.99629094513139E-5),
 .UNSPECIFIED.);
#200=B_SPLINE_CURVE_WITH_KNOTS('',3,(#23036,#23037,#23038,#23039),
 .UNSPECIFIED.,.F.,.F.,(4,4),(-0.310482170393536,-0.273153287835088),
 .UNSPECIFIED.);
#201=B_SPLINE_CURVE_WITH_KNOTS('',3,(#23040,#23041,#23042,#23043),
 .UNSPECIFIED.,.F.,.F.,(4,4),(0.273153287835088,0.310482170393536),
 .UNSPECIFIED.);
#202=B_SPLINE_CURVE_WITH_KNOTS('',3,(#23069,#23070,#23071,#23072,#23073,
#23074),.UNSPECIFIED.,.F.,.F.,(4,2,4),(-0.954291288267866,-0.799150016166134,
-0.681237813527804),.UNSPECIFIED.);
#203=B_SPLINE_CURVE_WITH_KNOTS('',3,(#23077,#23078,#23079,#23080,#23081,
#23082),.UNSPECIFIED.,.F.,.F.,(4,2,4),(0.681237813527804,0.799150016166134,
0.954291288267866),.UNSPECIFIED.);
#204=B_SPLINE_CURVE_WITH_KNOTS('',3,(#23099,#23100,#23101,#23102),
 .UNSPECIFIED.,.F.,.F.,(4,4),(-0.681237813527818,-0.643908930969367),
 .UNSPECIFIED.);
#205=B_SPLINE_CURVE_WITH_KNOTS('',3,(#23103,#23104,#23105,#23106),
 .UNSPECIFIED.,.F.,.F.,(4,4),(0.643908930969367,0.681237813527818),
 .UNSPECIFIED.);
#206=B_SPLINE_CURVE_WITH_KNOTS('',3,(#23111,#23112,#23113,#23114,#23115,
#23116),.UNSPECIFIED.,.F.,.F.,(4,2,4),(0.,0.155241085196768,0.310482170393536),
 .UNSPECIFIED.);
#207=B_SPLINE_CURVE_WITH_KNOTS('',3,(#23130,#23131,#23132,#23133,#23134,
#23135,#23136,#23137,#23138,#23139,#23140,#23141,#23142,#23143,#23144,#23145,
#23146,#23147,#23148,#23149,#23150,#23151,#23152,#23153,#23154,#23155,#23156,
#23157,#23158,#23159,#23160,#23161,#23162,#23163,#23164,#23165,#23166,#23167,
#23168,#23169,#23170,#23171,#23172,#23173,#23174,#23175,#23176,#23177,#23178,
#23179,#23180,#23181),.UNSPECIFIED.,.F.,.F.,(4,3,3,3,3,3,3,3,3,3,3,3,3,
3,3,3,3,4),(0.,0.0499444619143997,0.102213228836067,0.161337745961679,0.226027787112555,
0.322774313723485,0.388018393939231,0.444871191980803,0.498045966386616,
0.551308035462484,0.608971250191218,0.676370629650621,0.757277972237966,
0.819640071099801,0.876287931893757,0.929442916241627,0.979183143421037,
1.),.UNSPECIFIED.);
#208=B_SPLINE_CURVE_WITH_KNOTS('',3,(#23183,#23184,#23185,#23186),
 .UNSPECIFIED.,.F.,.F.,(4,4),(0.681229980645393,0.954283455385461),
 .UNSPECIFIED.);
#209=B_SPLINE_CURVE_WITH_KNOTS('',3,(#23188,#23189,#23190,#23191),
 .UNSPECIFIED.,.F.,.F.,(4,4),(0.64390109808696,0.681229980645406),
 .UNSPECIFIED.);
#210=B_SPLINE_CURVE_WITH_KNOTS('',3,(#23195,#23196,#23197,#23198),
 .UNSPECIFIED.,.F.,.F.,(4,4),(0.273153287835084,0.310482170393536),
 .UNSPECIFIED.);
#211=B_SPLINE_CURVE_WITH_KNOTS('',3,(#23200,#23201,#23202,#23203),
 .UNSPECIFIED.,.F.,.F.,(4,4),(9.9962909451316E-5,0.273153287835098),
 .UNSPECIFIED.);
#212=B_SPLINE_CURVE_WITH_KNOTS('',3,(#23204,#23205,#23206,#23207,#23208,
#23209,#23210,#23211,#23212,#23213,#23214,#23215,#23216,#23217,#23218,#23219,
#23220,#23221,#23222,#23223,#23224,#23225,#23226,#23227,#23228,#23229,#23230,
#23231,#23232,#23233,#23234,#23235,#23236,#23237,#23238,#23239,#23240,#23241,
#23242,#23243,#23244,#23245,#23246,#23247,#23248,#23249,#23250,#23251,#23252,
#23253,#23254,#23255),.UNSPECIFIED.,.F.,.F.,(4,3,3,3,3,3,3,3,3,3,3,3,3,
3,3,3,3,4),(0.,0.0499441833890994,0.102212663354842,0.161336814770156,0.226026300658892,
0.322773013076531,0.388016980146127,0.44486960598537,0.498043900535783,
0.551305760953592,0.608968431113942,0.676366602895863,0.757274952171898,
0.819637092644225,0.876284888158664,0.929439770311992,0.979179831894635,
1.),.UNSPECIFIED.);
#213=B_SPLINE_CURVE_WITH_KNOTS('',3,(#23278,#23279,#23280,#23281,#23282,
#23283,#23284,#23285,#23286,#23287,#23288,#23289,#23290,#23291,#23292,#23293,
#23294,#23295,#23296,#23297,#23298,#23299,#23300,#23301,#23302,#23303,#23304,
#23305,#23306,#23307,#23308,#23309,#23310,#23311,#23312,#23313,#23314,#23315,
#23316,#23317,#23318,#23319,#23320,#23321,#23322,#23323,#23324,#23325,#23326,
#23327,#23328,#23329,#23330,#23331,#23332,#23333,#23334,#23335,#23336,#23337,
#23338,#23339,#23340,#23341,#23342,#23343,#23344,#23345,#23346,#23347,#23348,
#23349,#23350,#23351,#23352,#23353,#23354,#23355,#23356,#23357,#23358,#23359),
 .UNSPECIFIED.,.F.,.F.,(4,3,3,3,3,3,3,3,3,3,3,3,3,3,3,3,3,3,3,3,3,3,3,3,
3,3,3,4),(0.,0.0295705059449982,0.0605159487132195,0.0926038163323903,0.126139587195106,
0.161619669086869,0.199971107221821,0.243460414815925,0.310976439628805,
0.354040412152005,0.394412886392504,0.42968604051999,0.462833625082738,
0.494651029536218,0.527129557597107,0.56064351985676,0.596019930404549,
0.634095034387078,0.676984118085056,0.757738088563792,0.79905173888368,
0.836280907354532,0.871099048793566,0.903485295079146,0.934889313990762,
0.965468175362615,0.99509132882554,1.),.UNSPECIFIED.);
#214=B_SPLINE_CURVE_WITH_KNOTS('',3,(#23361,#23362,#23363,#23364),
 .UNSPECIFIED.,.F.,.F.,(4,4),(-1.,0.),.UNSPECIFIED.);
#215=B_SPLINE_CURVE_WITH_KNOTS('',3,(#23366,#23367,#23368,#23369,#23370,
#23371,#23372,#23373,#23374,#23375,#23376,#23377,#23378,#23379,#23380,#23381,
#23382,#23383,#23384,#23385,#23386,#23387,#23388,#23389,#23390,#23391,#23392,
#23393,#23394,#23395,#23396,#23397,#23398,#23399,#23400,#23401,#23402,#23403,
#23404,#23405,#23406,#23407,#23408,#23409,#23410,#23411,#23412,#23413,#23414,
#23415,#23416,#23417),.UNSPECIFIED.,.F.,.F.,(4,3,3,3,3,3,3,3,3,3,3,3,3,
3,3,3,3,4),(0.,0.0499444620030573,0.102213229017714,0.161337746261311,0.226027787592192,
0.322774314143168,0.388018394389041,0.444871192483061,0.498045967040621,
0.551308036189455,0.608971251099731,0.676370630959906,0.757277973219929,
0.819640072069571,0.876287932886441,0.929442917270342,0.979183144505862,
1.),.UNSPECIFIED.);
#216=B_SPLINE_CURVE_WITH_KNOTS('',3,(#23457,#23458,#23459,#23460,#23461,
#23462,#23463,#23464,#23465,#23466,#23467,#23468,#23469,#23470,#23471,#23472,
#23473,#23474,#23475,#23476,#23477,#23478,#23479,#23480,#23481,#23482,#23483,
#23484,#23485,#23486,#23487,#23488,#23489,#23490,#23491,#23492,#23493,#23494,
#23495,#23496,#23497,#23498,#23499,#23500,#23501,#23502,#23503,#23504,#23505,
#23506,#23507,#23508),.UNSPECIFIED.,.F.,.F.,(4,3,3,3,3,3,3,3,3,3,3,3,3,
3,3,3,3,4),(0.,0.0499441826811105,0.102212661914011,0.161336812389129,0.226026296842565,
0.322773009737244,0.388016976561584,0.444869601982792,0.498043895325763,
0.551305755159944,0.608968423870338,0.676366592453702,0.757274944340276,
0.819637084909205,0.876284880238396,0.929439762109376,0.979179823244325,
1.),.UNSPECIFIED.);
#217=B_SPLINE_CURVE_WITH_KNOTS('',3,(#23510,#23511,#23512,#23513),
 .UNSPECIFIED.,.F.,.F.,(4,4),(0.,1.),.UNSPECIFIED.);
#218=B_SPLINE_CURVE_WITH_KNOTS('',3,(#23515,#23516,#23517,#23518,#23519,
#23520,#23521,#23522,#23523,#23524,#23525,#23526,#23527,#23528,#23529,#23530,
#23531,#23532,#23533,#23534,#23535,#23536,#23537,#23538,#23539,#23540,#23541,
#23542,#23543,#23544,#23545,#23546,#23547,#23548,#23549,#23550,#23551,#23552,
#23553,#23554,#23555,#23556,#23557,#23558,#23559,#23560,#23561,#23562,#23563,
#23564,#23565,#23566,#23567,#23568,#23569,#23570,#23571,#23572,#23573,#23574,
#23575,#23576,#23577,#23578,#23579,#23580,#23581,#23582,#23583,#23584,#23585,
#23586,#23587,#23588,#23589,#23590,#23591,#23592,#23593,#23594,#23595,#23596),
 .UNSPECIFIED.,.F.,.F.,(4,3,3,3,3,3,3,3,3,3,3,3,3,3,3,3,3,3,3,3,3,3,3,3,
3,3,3,4),(0.,0.0295773881131102,0.0605304169672427,0.0926266479882803,0.126171922795967,
0.161663359407986,0.20002975232552,0.243548698802509,0.31096187735372,0.354026760019112,
0.394400087517918,0.429679984520021,0.462839399606215,0.494661354039968,
0.527132669663605,0.560640871658796,0.596011154096698,0.63407950773218,
0.676959315385293,0.75771948653897,0.799022960211628,0.836244253893244,
0.871055469575763,0.903435210203173,0.934833075272608,0.965406057016351,
0.995023142060179,1.),.UNSPECIFIED.);
#219=B_SPLINE_CURVE_WITH_KNOTS('',3,(#23615,#23616,#23617,#23618),
 .UNSPECIFIED.,.F.,.F.,(4,4),(9.99629094513149E-5,0.273153287835104),
 .UNSPECIFIED.);
#220=B_SPLINE_CURVE_WITH_KNOTS('',3,(#23621,#23622,#23623,#23624),
 .UNSPECIFIED.,.F.,.F.,(4,4),(-0.273153287835104,-9.99629094513149E-5),
 .UNSPECIFIED.);
#221=B_SPLINE_CURVE_WITH_KNOTS('',3,(#23650,#23651,#23652,#23653),
 .UNSPECIFIED.,.F.,.F.,(4,4),(-0.310482170393536,-0.273153287835091),
 .UNSPECIFIED.);
#222=B_SPLINE_CURVE_WITH_KNOTS('',3,(#23654,#23655,#23656,#23657),
 .UNSPECIFIED.,.F.,.F.,(4,4),(0.273153287835091,0.310482170393536),
 .UNSPECIFIED.);
#223=B_SPLINE_CURVE_WITH_KNOTS('',3,(#23675,#23676,#23677,#23678),
 .UNSPECIFIED.,.F.,.F.,(4,4),(-0.954283455385459,-0.681229980645392),
 .UNSPECIFIED.);
#224=B_SPLINE_CURVE_WITH_KNOTS('',3,(#23681,#23682,#23683,#23684),
 .UNSPECIFIED.,.F.,.F.,(4,4),(0.681229980645392,0.954283455385459),
 .UNSPECIFIED.);
#225=B_SPLINE_CURVE_WITH_KNOTS('',3,(#23701,#23702,#23703,#23704),
 .UNSPECIFIED.,.F.,.F.,(4,4),(-0.681229980645406,-0.643901098086959),
 .UNSPECIFIED.);
#226=B_SPLINE_CURVE_WITH_KNOTS('',3,(#23705,#23706,#23707,#23708),
 .UNSPECIFIED.,.F.,.F.,(4,4),(0.643901098086959,0.681229980645406),
 .UNSPECIFIED.);
#227=B_SPLINE_CURVE_WITH_KNOTS('',3,(#23722,#23723,#23724,#23725,#23726,
#23727),.UNSPECIFIED.,.F.,.F.,(4,2,4),(0.643901098086957,0.799142183283726,
0.954383268480494),.UNSPECIFIED.);
#228=B_SPLINE_CURVE_WITH_KNOTS('',3,(#23757,#23758,#23759,#23760,#23761,
#23762,#23763,#23764,#23765,#23766,#23767,#23768,#23769,#23770,#23771,#23772,
#23773,#23774,#23775,#23776,#23777,#23778,#23779,#23780,#23781,#23782,#23783,
#23784,#23785,#23786,#23787,#23788,#23789,#23790,#23791,#23792,#23793,#23794,
#23795,#23796,#23797,#23798,#23799,#23800,#23801,#23802,#23803,#23804,#23805,
#23806,#23807,#23808,#23809,#23810,#23811,#23812,#23813,#23814,#23815,#23816,
#23817,#23818,#23819,#23820,#23821,#23822,#23823,#23824,#23825,#23826,#23827,
#23828,#23829,#23830,#23831,#23832,#23833,#23834,#23835,#23836,#23837,#23838),
 .UNSPECIFIED.,.F.,.F.,(4,3,3,3,3,3,3,3,3,3,3,3,3,3,3,3,3,3,3,3,3,3,3,3,
3,3,3,4),(0.,0.0295705059512633,0.0605159487271851,0.0926038163550416,0.126139587225611,
0.161619669126796,0.199971107275455,0.243460414898968,0.31097643981881,
0.354040412330134,0.394412886559501,0.429686040686443,0.46283362527423,
0.494651029717672,0.527129557769278,0.560643520045596,0.596019930614712,
0.634095034624437,0.676984118378702,0.757738088784027,0.799051739082071,
0.836280907545797,0.871099048983326,0.903485295270873,0.934889314183803,
0.965468175561812,0.995091329030122,1.),.UNSPECIFIED.);
#229=B_SPLINE_CURVE_WITH_KNOTS('',3,(#23839,#23840,#23841,#23842),
 .UNSPECIFIED.,.F.,.F.,(4,4),(-1.,0.),.UNSPECIFIED.);
#230=B_SPLINE_CURVE_WITH_KNOTS('',3,(#23881,#23882,#23883,#23884),
 .UNSPECIFIED.,.F.,.F.,(4,4),(0.,1.),.UNSPECIFIED.);
#231=B_SPLINE_CURVE_WITH_KNOTS('',3,(#23885,#23886,#23887,#23888,#23889,
#23890,#23891,#23892,#23893,#23894,#23895,#23896,#23897,#23898,#23899,#23900,
#23901,#23902,#23903,#23904,#23905,#23906,#23907,#23908,#23909,#23910,#23911,
#23912,#23913,#23914,#23915,#23916,#23917,#23918,#23919,#23920,#23921,#23922,
#23923,#23924,#23925,#23926,#23927,#23928,#23929,#23930,#23931,#23932,#23933,
#23934,#23935,#23936,#23937,#23938,#23939,#23940,#23941,#23942,#23943,#23944,
#23945,#23946,#23947,#23948,#23949,#23950,#23951,#23952,#23953,#23954,#23955,
#23956,#23957,#23958,#23959,#23960,#23961,#23962,#23963,#23964,#23965,#23966),
 .UNSPECIFIED.,.F.,.F.,(4,3,3,3,3,3,3,3,3,3,3,3,3,3,3,3,3,3,3,3,3,3,3,3,
3,3,3,4),(0.,0.0295773880524302,0.0605304168410243,0.092626647792498,0.126171922525243,
0.161663359050634,0.200029751864124,0.24354869819935,0.31096188049952,0.3540267629683,
0.394400090282781,0.429679987033957,0.462839402284777,0.494661356438073,
0.527132671762529,0.560640873794645,0.59601115629688,0.634079510052112,
0.676959318040989,0.757719488530741,0.799022961866045,0.836244255350966,
0.871055470885213,0.903435211410382,0.934833076388468,0.965406058048494,
0.995023143024151,1.),.UNSPECIFIED.);
#232=B_SPLINE_CURVE_WITH_KNOTS('',3,(#23985,#23986,#23987,#23988),
 .UNSPECIFIED.,.F.,.F.,(4,4),(-0.273153287835098,-9.9962909451316E-5),
 .UNSPECIFIED.);
#233=B_SPLINE_CURVE_WITH_KNOTS('',3,(#24011,#24012,#24013,#24014),
 .UNSPECIFIED.,.F.,.F.,(4,4),(-0.310482170393536,-0.273153287835084),
 .UNSPECIFIED.);
#234=B_SPLINE_CURVE_WITH_KNOTS('',3,(#24032,#24033,#24034,#24035),
 .UNSPECIFIED.,.F.,.F.,(4,4),(-0.954283455385461,-0.681229980645393),
 .UNSPECIFIED.);
#235=B_SPLINE_CURVE_WITH_KNOTS('',3,(#24053,#24054,#24055,#24056),
 .UNSPECIFIED.,.F.,.F.,(4,4),(-0.681229980645406,-0.64390109808696),
 .UNSPECIFIED.);
#236=B_SPLINE_CURVE_WITH_KNOTS('',3,(#24061,#24062,#24063,#24064,#24065,
#24066,#24067,#24068,#24069,#24070,#24071,#24072,#24073,#24074,#24075,#24076,
#24077,#24078,#24079,#24080,#24081,#24082,#24083,#24084,#24085,#24086,#24087,
#24088,#24089,#24090,#24091,#24092,#24093,#24094,#24095,#24096,#24097,#24098,
#24099,#24100,#24101,#24102,#24103,#24104,#24105,#24106,#24107,#24108,#24109,
#24110,#24111,#24112,#24113,#24114,#24115,#24116,#24117,#24118,#24119,#24120,
#24121,#24122,#24123,#24124,#24125,#24126,#24127,#24128,#24129,#24130,#24131,
#24132,#24133,#24134,#24135,#24136,#24137,#24138,#24139,#24140,#24141,#24142),
 .UNSPECIFIED.,.F.,.F.,(4,3,3,3,3,3,3,3,3,3,3,3,3,3,3,3,3,3,3,3,3,3,3,3,
3,3,3,4),(0.,0.029577388096564,0.0605304169342327,0.092626647938075,0.126171922726201,
0.161663359317722,0.200029752207105,0.243548698650945,0.310961878143349,
0.354026760759389,0.394400088211927,0.42967998515154,0.462839400279756,
0.49466135464192,0.527132670190963,0.560640872195637,0.596011154650127,
0.634079508317272,0.676959316055784,0.757719487041838,0.799022960628449,
0.836244254262571,0.871055469905186,0.903435210506207,0.934833075552335,
0.965406057277606,0.995023142305148,1.),.UNSPECIFIED.);
#237=B_SPLINE_CURVE_WITH_KNOTS('',3,(#24144,#24145,#24146,#24147),
 .UNSPECIFIED.,.F.,.F.,(4,4),(-0.273153287835103,-9.99629094513129E-5),
 .UNSPECIFIED.);
#238=B_SPLINE_CURVE_WITH_KNOTS('',3,(#24175,#24176,#24177,#24178,#24179,
#24180,#24181,#24182,#24183,#24184,#24185,#24186,#24187,#24188,#24189,#24190,
#24191,#24192,#24193,#24194,#24195,#24196,#24197,#24198,#24199,#24200,#24201,
#24202,#24203,#24204,#24205,#24206,#24207,#24208,#24209,#24210,#24211,#24212,
#24213,#24214,#24215,#24216,#24217,#24218,#24219,#24220,#24221,#24222,#24223,
#24224,#24225,#24226,#24227,#24228,#24229,#24230,#24231,#24232,#24233,#24234,
#24235,#24236,#24237,#24238,#24239,#24240,#24241,#24242,#24243,#24244,#24245,
#24246,#24247,#24248,#24249,#24250,#24251,#24252,#24253,#24254,#24255,#24256),
 .UNSPECIFIED.,.F.,.F.,(4,3,3,3,3,3,3,3,3,3,3,3,3,3,3,3,3,3,3,3,3,3,3,3,
3,3,3,4),(0.,0.0295705059230571,0.0605159486675307,0.0926038162612098,0.126139587094081,
0.161619668951887,0.199971107044072,0.243460414557264,0.310976439007079,
0.354040411569137,0.394412885846066,0.429686039982072,0.462833624458263,
0.494651028937512,0.527129557030697,0.560643519234331,0.596019929713393,
0.634095033602269,0.676984117126932,0.757738087845199,0.799051738231756,
0.836280906723594,0.871099048170336,0.903485294450174,0.934889313352345,
0.965468174717861,0.99509132816655,1.),.UNSPECIFIED.);
#239=B_SPLINE_CURVE_WITH_KNOTS('',3,(#24258,#24259,#24260,#24261),
 .UNSPECIFIED.,.F.,.F.,(4,4),(-1.,0.),.UNSPECIFIED.);
#240=B_SPLINE_CURVE_WITH_KNOTS('',3,(#24262,#24263,#24264,#24265,#24266,
#24267,#24268,#24269,#24270,#24271,#24272,#24273,#24274,#24275,#24276,#24277,
#24278,#24279,#24280,#24281,#24282,#24283,#24284,#24285,#24286,#24287,#24288,
#24289,#24290,#24291,#24292,#24293,#24294,#24295,#24296,#24297,#24298,#24299,
#24300,#24301,#24302,#24303,#24304,#24305,#24306,#24307,#24308,#24309,#24310,
#24311,#24312,#24313),.UNSPECIFIED.,.F.,.F.,(4,3,3,3,3,3,3,3,3,3,3,3,3,
3,3,3,3,4),(0.,0.0499444622913127,0.102213229603,0.161337747229144,0.226027789144532,
0.322774315501466,0.388018395848148,0.444871194112166,0.498045969161075,
0.551308038547837,0.60897125404869,0.676370635211665,0.757277976408749,
0.81964007521899,0.876287936111462,0.92944292060967,0.979183148027608,1.),
 .UNSPECIFIED.);
#241=B_SPLINE_CURVE_WITH_KNOTS('',3,(#24351,#24352,#24353,#24354,#24355,
#24356,#24357,#24358,#24359,#24360,#24361,#24362,#24363,#24364,#24365,#24366,
#24367,#24368,#24369,#24370,#24371,#24372,#24373,#24374,#24375,#24376,#24377,
#24378,#24379,#24380,#24381,#24382,#24383,#24384,#24385,#24386,#24387,#24388,
#24389,#24390,#24391,#24392,#24393,#24394,#24395,#24396,#24397,#24398,#24399,
#24400,#24401,#24402),.UNSPECIFIED.,.F.,.F.,(4,3,3,3,3,3,3,3,3,3,3,3,3,
3,3,3,3,4),(0.,0.0499441828589668,0.102212662275513,0.161336812986304,0.226026297799104,
0.322773010574216,0.388016977460993,0.444869602986684,0.498043896631638,
0.551305756611869,0.608968425686129,0.676366595071555,0.757274946303666,
0.819637086848271,0.876284882223587,0.929439764165566,0.979179825412561,
1.),.UNSPECIFIED.);
#242=B_SPLINE_CURVE_WITH_KNOTS('',3,(#24403,#24404,#24405,#24406),
 .UNSPECIFIED.,.F.,.F.,(4,4),(0.,1.),.UNSPECIFIED.);
#243=B_SPLINE_CURVE_WITH_KNOTS('',3,(#24424,#24425,#24426,#24427),
 .UNSPECIFIED.,.F.,.F.,(4,4),(9.99629094513129E-5,0.273153287835103),
 .UNSPECIFIED.);
#244=B_SPLINE_CURVE_WITH_KNOTS('',3,(#24454,#24455,#24456,#24457),
 .UNSPECIFIED.,.F.,.F.,(4,4),(-0.310482170393537,-0.273153287835089),
 .UNSPECIFIED.);
#245=B_SPLINE_CURVE_WITH_KNOTS('',3,(#24458,#24459,#24460,#24461),
 .UNSPECIFIED.,.F.,.F.,(4,4),(0.273153287835089,0.310482170393537),
 .UNSPECIFIED.);
#246=B_SPLINE_CURVE_WITH_KNOTS('',3,(#24479,#24480,#24481,#24482),
 .UNSPECIFIED.,.F.,.F.,(4,4),(-0.95428345538546,-0.681229980645392),
 .UNSPECIFIED.);
#247=B_SPLINE_CURVE_WITH_KNOTS('',3,(#24485,#24486,#24487,#24488),
 .UNSPECIFIED.,.F.,.F.,(4,4),(0.681229980645392,0.95428345538546),
 .UNSPECIFIED.);
#248=B_SPLINE_CURVE_WITH_KNOTS('',3,(#24505,#24506,#24507,#24508),
 .UNSPECIFIED.,.F.,.F.,(4,4),(-0.681229980645405,-0.643901098086959),
 .UNSPECIFIED.);
#249=B_SPLINE_CURVE_WITH_KNOTS('',3,(#24509,#24510,#24511,#24512),
 .UNSPECIFIED.,.F.,.F.,(4,4),(0.643901098086959,0.681229980645405),
 .UNSPECIFIED.);
#250=B_SPLINE_CURVE_WITH_KNOTS('',3,(#24526,#24527,#24528,#24529,#24530,
#24531),.UNSPECIFIED.,.F.,.F.,(4,2,4),(0.,0.155241085196768,0.310482170393536),
 .UNSPECIFIED.);
#251=B_SPLINE_CURVE_WITH_KNOTS('',3,(#24534,#24535,#24536,#24537,#24538,
#24539),.UNSPECIFIED.,.F.,.F.,(4,2,4),(0.,0.155241085196768,0.310482170393535),
 .UNSPECIFIED.);
#252=B_SPLINE_CURVE_WITH_KNOTS('',3,(#24542,#24543,#24544,#24545,#24546,
#24547),.UNSPECIFIED.,.F.,.F.,(4,2,4),(0.643908930969365,0.799150016166132,
0.9543911013629),.UNSPECIFIED.);
#253=B_SPLINE_CURVE_WITH_KNOTS('',3,(#24550,#24551,#24552,#24553,#24554,
#24555),.UNSPECIFIED.,.F.,.F.,(4,2,4),(0.,0.15524108519677,0.310482170393539),
 .UNSPECIFIED.);
#254=B_SPLINE_CURVE_WITH_KNOTS('',3,(#24560,#24561,#24562,#24563,#24564,
#24565),.UNSPECIFIED.,.F.,.F.,(4,2,4),(0.643908930969368,0.799150016166137,
0.954391101362907),.UNSPECIFIED.);
#255=B_SPLINE_CURVE_WITH_KNOTS('',3,(#24566,#24567,#24568,#24569,#24570,
#24571),.UNSPECIFIED.,.F.,.F.,(4,2,4),(0.643908930969366,0.799150016166134,
0.954391101362902),.UNSPECIFIED.);
#256=B_SPLINE_CURVE_WITH_KNOTS('',3,(#24603,#24604,#24605,#24606,#24607,
#24608,#24609,#24610,#24611,#24612,#24613,#24614,#24615,#24616,#24617,#24618,
#24619,#24620,#24621,#24622,#24623,#24624,#24625,#24626,#24627,#24628,#24629,
#24630,#24631,#24632,#24633,#24634,#24635,#24636,#24637,#24638,#24639,#24640,
#24641,#24642,#24643,#24644,#24645,#24646,#24647,#24648),.UNSPECIFIED.,
 .F.,.F.,(4,3,3,3,3,3,3,3,3,3,3,3,3,3,3,4),(0.,0.0572017311997757,0.120330894890292,
0.190833525219608,0.280000607593217,0.370000531644065,0.437396979145379,
0.498588004507602,0.56260087801746,0.634065239574647,0.727489847395828,
0.803842080523512,0.870326860317577,0.931777978339434,0.988871097236517,
1.),.UNSPECIFIED.);
#257=B_SPLINE_CURVE_WITH_KNOTS('',3,(#24650,#24651,#24652,#24653),
 .UNSPECIFIED.,.F.,.F.,(4,4),(-1.,0.),.UNSPECIFIED.);
#258=B_SPLINE_CURVE_WITH_KNOTS('',3,(#24655,#24656,#24657,#24658,#24659,
#24660,#24661,#24662,#24663,#24664,#24665,#24666,#24667,#24668,#24669,#24670,
#24671,#24672,#24673,#24674,#24675,#24676,#24677,#24678,#24679,#24680,#24681,
#24682,#24683,#24684,#24685,#24686,#24687,#24688,#24689,#24690,#24691,#24692,
#24693,#24694,#24695,#24696,#24697,#24698,#24699,#24700),.UNSPECIFIED.,
 .F.,.F.,(4,3,3,3,3,3,3,3,3,3,3,3,3,3,3,4),(0.,0.057203025224468,0.120333802338101,
0.190838689067532,0.280011837452007,0.370010357770506,0.437406670172117,
0.498598114794378,0.562610573319897,0.63407537003659,0.727505599643409,
0.803852814253569,0.870334971678201,0.931784146571509,0.988875797228613,
1.),.UNSPECIFIED.);
#259=B_SPLINE_CURVE_WITH_KNOTS('',3,(#24728,#24729,#24730,#24731,#24732,
#24733,#24734,#24735,#24736,#24737,#24738,#24739,#24740,#24741,#24742,#24743,
#24744,#24745,#24746,#24747,#24748,#24749,#24750,#24751,#24752,#24753,#24754,
#24755,#24756,#24757,#24758,#24759,#24760,#24761,#24762,#24763,#24764,#24765,
#24766,#24767,#24768,#24769,#24770,#24771,#24772,#24773),.UNSPECIFIED.,
 .F.,.F.,(4,3,3,3,3,3,3,3,3,3,3,3,3,3,3,4),(0.,0.0572017312000063,0.120330894890857,
0.190833525220496,0.280000607590238,0.370000531641458,0.437396979143437,
0.498588004432005,0.562600877937054,0.634065239482155,0.727489847253419,
0.803842080404544,0.870326860202434,0.931777978231419,0.98887109713731,
1.),.UNSPECIFIED.);
#260=B_SPLINE_CURVE_WITH_KNOTS('',3,(#24775,#24776,#24777,#24778),
 .UNSPECIFIED.,.F.,.F.,(4,4),(0.,1.),.UNSPECIFIED.);
#261=B_SPLINE_CURVE_WITH_KNOTS('',3,(#24780,#24781,#24782,#24783,#24784,
#24785,#24786,#24787,#24788,#24789,#24790,#24791,#24792,#24793,#24794,#24795,
#24796,#24797,#24798,#24799,#24800,#24801,#24802,#24803,#24804,#24805,#24806,
#24807,#24808,#24809,#24810,#24811,#24812,#24813,#24814,#24815,#24816,#24817,
#24818,#24819,#24820,#24821,#24822,#24823,#24824,#24825),.UNSPECIFIED.,
 .F.,.F.,(4,3,3,3,3,3,3,3,3,3,3,3,3,3,3,4),(0.,0.0572030252319667,0.120333802345375,
0.190838689076385,0.280011837453422,0.370010357771744,0.437406670174618,
0.498598114865344,0.562610573396659,0.634075370121406,0.727505599797859,
0.803852814376215,0.870334971791533,0.931784146677532,0.988875797332666,
1.),.UNSPECIFIED.);
#262=B_SPLINE_CURVE_WITH_KNOTS('',3,(#24852,#24853,#24854,#24855,#24856,
#24857),.UNSPECIFIED.,.F.,.F.,(4,1,1,4),(-1.70953476876622,-0.976877010723551,
-0.48843850536177,1.11854969730985E-14),.UNSPECIFIED.);
#263=B_SPLINE_CURVE_WITH_KNOTS('',3,(#24860,#24861,#24862,#24863,#24864,
#24865),.UNSPECIFIED.,.F.,.F.,(4,1,1,4),(-1.11854969730985E-14,0.48843850536177,
0.976877010723551,1.70953476876622),.UNSPECIFIED.);
#264=B_SPLINE_CURVE_WITH_KNOTS('',3,(#24900,#24901,#24902,#24903,#24904,
#24905,#24906),.UNSPECIFIED.,.F.,.F.,(4,1,1,1,4),(1.43205788482356,1.92049639018535,
2.40893489554713,2.77526377456847,3.1415926535898),.UNSPECIFIED.);
#265=B_SPLINE_CURVE_WITH_KNOTS('',3,(#24907,#24908,#24909,#24910,#24911,
#24912,#24913),.UNSPECIFIED.,.F.,.F.,(4,1,1,1,4),(-3.1415926535898,-2.77526377456847,
-2.40893489554713,-1.92049639018535,-1.43205788482356),.UNSPECIFIED.);
#266=B_SPLINE_CURVE_WITH_KNOTS('',3,(#24932,#24933,#24934,#24935,#24936,
#24937),.UNSPECIFIED.,.F.,.F.,(4,1,1,4),(-1.70953476876624,-0.976877010723567,
-0.488438505361783,0.),.UNSPECIFIED.);
#267=B_SPLINE_CURVE_WITH_KNOTS('',3,(#24938,#24939,#24940,#24941,#24942,
#24943,#24944,#24945,#24946,#24947,#24948,#24949,#24950,#24951,#24952,#24953,
#24954,#24955,#24956,#24957,#24958,#24959,#24960,#24961,#24962,#24963,#24964,
#24965,#24966,#24967,#24968,#24969,#24970,#24971,#24972,#24973,#24974,#24975,
#24976,#24977,#24978,#24979,#24980,#24981,#24982,#24983),.UNSPECIFIED.,
 .F.,.F.,(4,3,3,3,3,3,3,3,3,3,3,3,3,3,3,4),(0.,0.0572017311994344,0.120330894888931,
0.19083352521961,0.28000060759744,0.37000053164776,0.437396979149183,0.498588004127736,
0.562600877612139,0.634065239106159,0.727489846545216,0.803842079829981,
0.870326859689392,0.93177797774672,0.988871096661088,1.),.UNSPECIFIED.);
#268=B_SPLINE_CURVE_WITH_KNOTS('',3,(#24992,#24993,#24994,#24995,#24996,
#24997,#24998,#24999,#25000,#25001,#25002,#25003,#25004,#25005,#25006,#25007,
#25008,#25009,#25010,#25011,#25012,#25013,#25014,#25015,#25016,#25017,#25018,
#25019,#25020,#25021,#25022,#25023,#25024,#25025,#25026,#25027,#25028,#25029,
#25030,#25031,#25032,#25033,#25034,#25035,#25036,#25037),.UNSPECIFIED.,
 .F.,.F.,(4,3,3,3,3,3,3,3,3,3,3,3,3,3,3,4),(0.,0.0572030252313222,0.120333802345085,
0.190838689078026,0.280011837457414,0.370010357775237,0.437406670179801,
0.498598114642262,0.562610573159454,0.634075369847749,0.727505599310812,
0.803852813978605,0.870334971432735,0.931784146343715,0.988875797008993,
1.),.UNSPECIFIED.);
#269=B_SPLINE_CURVE_WITH_KNOTS('',3,(#25038,#25039,#25040,#25041,#25042,
#25043),.UNSPECIFIED.,.F.,.F.,(4,1,1,4),(0.,0.488438505361777,0.976877010723555,
1.70953476876622),.UNSPECIFIED.);
#270=B_SPLINE_CURVE_WITH_KNOTS('',3,(#25070,#25071,#25072,#25073,#25074,
#25075,#25076,#25077,#25078,#25079,#25080,#25081,#25082,#25083,#25084,#25085,
#25086,#25087,#25088,#25089,#25090,#25091,#25092,#25093,#25094,#25095,#25096,
#25097,#25098,#25099,#25100,#25101,#25102,#25103,#25104,#25105,#25106,#25107,
#25108,#25109,#25110,#25111,#25112,#25113,#25114,#25115),.UNSPECIFIED.,
 .F.,.F.,(4,3,3,3,3,3,3,3,3,3,3,3,3,3,3,4),(0.,0.0572017311976094,0.120330894887026,
0.190833525221234,0.280000607599086,0.3700005316492,0.437396979153787,0.498588004443689,
0.562600877950485,0.634065239495553,0.727489847237366,0.803842080393393,
0.87032686020045,0.931777978227553,0.988871097128439,1.),.UNSPECIFIED.);
#271=B_SPLINE_CURVE_WITH_KNOTS('',3,(#25116,#25117,#25118,#25119),
 .UNSPECIFIED.,.F.,.F.,(4,4),(0.,1.),.UNSPECIFIED.);
#272=B_SPLINE_CURVE_WITH_KNOTS('',3,(#25146,#25147,#25148,#25149),
 .UNSPECIFIED.,.F.,.F.,(4,4),(0.,1.),.UNSPECIFIED.);
#273=B_SPLINE_CURVE_WITH_KNOTS('',3,(#25150,#25151,#25152,#25153,#25154,
#25155,#25156,#25157,#25158,#25159,#25160,#25161,#25162,#25163,#25164,#25165,
#25166,#25167,#25168,#25169,#25170,#25171,#25172,#25173,#25174,#25175,#25176,
#25177,#25178,#25179,#25180,#25181,#25182,#25183,#25184,#25185,#25186,#25187,
#25188,#25189,#25190,#25191,#25192,#25193,#25194,#25195),.UNSPECIFIED.,
 .F.,.F.,(4,3,3,3,3,3,3,3,3,3,3,3,3,3,3,4),(0.,0.0572030252324622,0.120333802346723,
0.190838689076922,0.280011837457471,0.370010357775287,0.437406670183435,
0.498598114641987,0.562610573159151,0.634075369845933,0.727505599300381,
0.803852813971137,0.870334971421258,0.931784146332158,0.988875796999179,
1.),.UNSPECIFIED.);
#274=B_SPLINE_CURVE_WITH_KNOTS('',3,(#25222,#25223,#25224,#25225,#25226,
#25227),.UNSPECIFIED.,.F.,.F.,(4,1,1,4),(0.,0.488438505361783,0.976877010723567,
1.70953476876624),.UNSPECIFIED.);
#275=B_SPLINE_CURVE_WITH_KNOTS('',3,(#25256,#25257,#25258,#25259,#25260,
#25261),.UNSPECIFIED.,.F.,.F.,(4,1,1,4),(-1.70953476876622,-0.976877010723555,
-0.488438505361777,0.),.UNSPECIFIED.);
#276=B_SPLINE_CURVE_WITH_KNOTS('',3,(#25287,#25288,#25289,#25290,#25291,
#25292,#25293,#25294,#25295,#25296,#25297,#25298,#25299,#25300,#25301,#25302,
#25303,#25304,#25305,#25306,#25307,#25308,#25309,#25310,#25311,#25312,#25313,
#25314,#25315,#25316,#25317,#25318,#25319,#25320,#25321,#25322,#25323,#25324,
#25325,#25326,#25327,#25328,#25329,#25330,#25331,#25332),.UNSPECIFIED.,
 .F.,.F.,(4,3,3,3,3,3,3,3,3,3,3,3,3,3,3,4),(0.,0.0572017311991183,0.120330894889653,
0.190833525219955,0.280000607594411,0.37000053164511,0.437396979144203,
0.498588004649256,0.56260087816826,0.634065239749291,0.727489847706123,
0.803842080776209,0.870326860547973,0.931777978552727,0.988871097444316,
1.),.UNSPECIFIED.);
#277=B_SPLINE_CURVE_WITH_KNOTS('',3,(#25334,#25335,#25336,#25337),
 .UNSPECIFIED.,.F.,.F.,(4,4),(0.,1.),.UNSPECIFIED.);
#278=B_SPLINE_CURVE_WITH_KNOTS('',3,(#25338,#25339,#25340,#25341,#25342,
#25343,#25344,#25345,#25346,#25347,#25348,#25349,#25350,#25351,#25352,#25353,
#25354,#25355,#25356,#25357,#25358,#25359,#25360,#25361,#25362,#25363,#25364,
#25365,#25366,#25367,#25368,#25369,#25370,#25371,#25372,#25373,#25374,#25375,
#25376,#25377,#25378,#25379,#25380,#25381,#25382,#25383),.UNSPECIFIED.,
 .F.,.F.,(4,3,3,3,3,3,3,3,3,3,3,3,3,3,3,4),(0.,0.0572030252343024,0.12033380234866,
0.190838689076873,0.280011837448138,0.370010357767121,0.437406670172275,
0.498598114697011,0.562610573216881,0.634075369917583,0.727505599449089,
0.803852814091775,0.870334971532607,0.931784146442687,0.988875797099411,
1.),.UNSPECIFIED.);
#279=B_SPLINE_CURVE_WITH_KNOTS('',3,(#25410,#25411,#25412,#25413,#25414,
#25415,#25416,#25417,#25418,#25419,#25420,#25421,#25422,#25423,#25424,#25425,
#25426,#25427,#25428,#25429,#25430,#25431,#25432,#25433,#25434,#25435,#25436,
#25437,#25438,#25439,#25440,#25441,#25442,#25443,#25444,#25445,#25446,#25447,
#25448,#25449,#25450,#25451,#25452,#25453,#25454,#25455),.UNSPECIFIED.,
 .F.,.F.,(4,3,3,3,3,3,3,3,3,3,3,3,3,3,3,4),(0.,0.0572017312009936,0.120330894888744,
0.190833525225305,0.280000607597786,0.370000531648063,0.437396979151322,
0.49858800483577,0.562600878367579,0.634065239978569,0.727489848107998,
0.8038420811056,0.870326860843456,0.931777978817204,0.988871097702708,1.),
 .UNSPECIFIED.);
#280=B_SPLINE_CURVE_WITH_KNOTS('',3,(#25457,#25458,#25459,#25460),
 .UNSPECIFIED.,.F.,.F.,(4,4),(0.,1.),.UNSPECIFIED.);
#281=B_SPLINE_CURVE_WITH_KNOTS('',3,(#25462,#25463,#25464,#25465,#25466,
#25467,#25468,#25469,#25470,#25471,#25472,#25473,#25474,#25475,#25476,#25477,
#25478,#25479,#25480,#25481,#25482,#25483,#25484,#25485,#25486,#25487,#25488,
#25489,#25490,#25491,#25492,#25493,#25494,#25495,#25496,#25497,#25498,#25499,
#25500,#25501,#25502,#25503,#25504,#25505,#25506,#25507),.UNSPECIFIED.,
 .F.,.F.,(4,3,3,3,3,3,3,3,3,3,3,3,3,3,3,4),(0.,0.0572030252317164,0.120333802345145,
0.19083868907559,0.280011837455817,0.37001035777384,0.437406670175968,0.498598114641638,
0.562610573158253,0.634075369846188,0.727505599314327,0.803852813981206,
0.870334971433397,0.93178414634131,0.98887579700713,1.),.UNSPECIFIED.);
#282=B_SPLINE_CURVE_WITH_KNOTS('',3,(#25534,#25535,#25536,#25537,#25538,
#25539),.UNSPECIFIED.,.F.,.F.,(4,1,1,4),(-1.70953476876621,-0.976877010723542,
-0.48843850536176,2.22044604925035E-14),.UNSPECIFIED.);
#283=B_SPLINE_CURVE_WITH_KNOTS('',3,(#25542,#25543,#25544,#25545,#25546,
#25547),.UNSPECIFIED.,.F.,.F.,(4,1,1,4),(-2.22044604925035E-14,0.48843850536176,
0.976877010723542,1.70953476876621),.UNSPECIFIED.);
#284=B_SPLINE_CURVE_WITH_KNOTS('',3,(#25578,#25579,#25580,#25581,#25582,
#25583),.UNSPECIFIED.,.F.,.F.,(4,1,1,4),(-1.70953476876621,-0.97687701072354,
-0.488438505361759,2.22044604925031E-14),.UNSPECIFIED.);
#285=B_SPLINE_CURVE_WITH_KNOTS('',3,(#25584,#25585,#25586,#25587,#25588,
#25589),.UNSPECIFIED.,.F.,.F.,(4,1,1,4),(-2.22044604925031E-14,0.488438505361759,
0.97687701072354,1.70953476876621),.UNSPECIFIED.);
#286=B_SPLINE_CURVE_WITH_KNOTS('',3,(#25594,#25595,#25596,#25597,#25598,
#25599),.UNSPECIFIED.,.F.,.F.,(4,1,1,4),(-1.70953476876623,-0.976877010723559,
-0.488438505361781,-2.77555756156289E-15),.UNSPECIFIED.);
#287=B_SPLINE_CURVE_WITH_KNOTS('',3,(#25600,#25601,#25602,#25603,#25604,
#25605,#25606,#25607,#25608,#25609,#25610,#25611,#25612,#25613,#25614,#25615,
#25616,#25617,#25618,#25619,#25620,#25621,#25622,#25623,#25624,#25625,#25626,
#25627,#25628,#25629,#25630,#25631,#25632,#25633,#25634,#25635,#25636,#25637,
#25638,#25639,#25640,#25641,#25642,#25643,#25644,#25645),.UNSPECIFIED.,
 .F.,.F.,(4,3,3,3,3,3,3,3,3,3,3,3,3,3,3,4),(0.,0.0572017311987612,0.120330894889715,
0.190833525218877,0.280000607593098,0.370000531643961,0.437396979144952,
0.498588004371557,0.562600877871927,0.634065239405833,0.727489847083102,
0.803842080268102,0.870326860085879,0.931777978122396,0.988871097026644,
1.),.UNSPECIFIED.);
#288=B_SPLINE_CURVE_WITH_KNOTS('',3,(#25654,#25655,#25656,#25657,#25658,
#25659,#25660,#25661,#25662,#25663,#25664,#25665,#25666,#25667,#25668,#25669,
#25670,#25671,#25672,#25673,#25674,#25675,#25676,#25677,#25678,#25679,#25680,
#25681,#25682,#25683,#25684,#25685,#25686,#25687,#25688,#25689,#25690,#25691,
#25692,#25693,#25694,#25695,#25696,#25697,#25698,#25699),.UNSPECIFIED.,
 .F.,.F.,(4,3,3,3,3,3,3,3,3,3,3,3,3,3,3,4),(0.,0.0572030252318266,0.120333802345496,
0.190838689075676,0.280011837456741,0.370010357774648,0.437406670177162,
0.498598114850172,0.562610573381775,0.634075370104953,0.727505599770209,
0.803852814352912,0.870334971770891,0.9317841466576,0.988875797314384,1.),
 .UNSPECIFIED.);
#289=B_SPLINE_CURVE_WITH_KNOTS('',3,(#25700,#25701,#25702,#25703,#25704,
#25705),.UNSPECIFIED.,.F.,.F.,(4,1,1,4),(2.77555756156289E-15,0.488438505361782,
0.976877010723562,1.70953476876623),.UNSPECIFIED.);
#290=B_SPLINE_CURVE_WITH_KNOTS('',3,(#25736,#25737,#25738,#25739),
 .UNSPECIFIED.,.F.,.F.,(4,4),(0.,1.),.UNSPECIFIED.);
#291=B_SPLINE_CURVE_WITH_KNOTS('',3,(#25740,#25741,#25742,#25743,#25744,
#25745,#25746,#25747,#25748,#25749,#25750,#25751,#25752,#25753,#25754,#25755,
#25756,#25757,#25758,#25759,#25760,#25761,#25762,#25763,#25764,#25765,#25766,
#25767,#25768,#25769,#25770,#25771,#25772,#25773,#25774,#25775,#25776,#25777,
#25778,#25779,#25780,#25781,#25782,#25783,#25784,#25785),.UNSPECIFIED.,
 .F.,.F.,(4,3,3,3,3,3,3,3,3,3,3,3,3,3,3,4),(0.,0.0572030252318119,0.120333802345044,
0.190838689074226,0.280011837457671,0.370010357775463,0.437406670175368,
0.498598114719374,0.562610573241369,0.634075369941395,0.727505599476499,
0.803852814114293,0.870334971552934,0.931784146453147,0.98887579711519,
1.),.UNSPECIFIED.);
#292=B_SPLINE_CURVE_WITH_KNOTS('',3,(#25811,#25812,#25813,#25814,#25815,
#25816,#25817,#25818,#25819,#25820,#25821,#25822,#25823,#25824,#25825,#25826,
#25827,#25828,#25829,#25830,#25831,#25832,#25833,#25834,#25835,#25836,#25837,
#25838,#25839,#25840,#25841,#25842,#25843,#25844,#25845,#25846,#25847,#25848,
#25849,#25850,#25851,#25852,#25853,#25854,#25855,#25856),.UNSPECIFIED.,
 .F.,.F.,(4,3,3,3,3,3,3,3,3,3,3,3,3,3,3,4),(0.,0.0572017311987599,0.120330894889451,
0.190833525224185,0.28000060760209,0.370000531651829,0.437396979150436,
0.498588004343821,0.562600877842339,0.63406523937154,0.727489847024129,
0.803842080219329,0.870326860044885,0.931777978082536,0.988871096986048,
1.),.UNSPECIFIED.);
#293=B_SPLINE_CURVE_WITH_KNOTS('',3,(#25857,#25858,#25859,#25860),
 .UNSPECIFIED.,.F.,.F.,(4,4),(0.,1.),.UNSPECIFIED.);
#294=B_SPLINE_CURVE_WITH_KNOTS('',3,(#25886,#25887,#25888,#25889,#25890,
#25891),.UNSPECIFIED.,.F.,.F.,(4,1,1,4),(-1.70953476876623,-0.976877010723562,
-0.488438505361782,-2.77555756156289E-15),.UNSPECIFIED.);
#295=B_SPLINE_CURVE_WITH_KNOTS('',3,(#25921,#25922,#25923,#25924,#25925,
#25926),.UNSPECIFIED.,.F.,.F.,(4,1,1,4),(2.77555756156289E-15,0.488438505361781,
0.976877010723559,1.70953476876623),.UNSPECIFIED.);
#296=B_SPLINE_CURVE_WITH_KNOTS('',3,(#27048,#27049,#27050,#27051,#27052,
#27053,#27054,#27055,#27056,#27057,#27058,#27059,#27060,#27061,#27062,#27063,
#27064,#27065,#27066,#27067,#27068,#27069,#27070,#27071,#27072,#27073,#27074,
#27075,#27076,#27077,#27078,#27079,#27080,#27081,#27082,#27083,#27084,#27085,
#27086,#27087,#27088,#27089,#27090,#27091,#27092,#27093,#27094,#27095,#27096,
#27097,#27098,#27099,#27100,#27101,#27102,#27103,#27104,#27105,#27106,#27107,
#27108,#27109,#27110,#27111,#27112,#27113,#27114),.UNSPECIFIED.,.F.,.F.,
(4,3,3,3,3,3,3,3,3,3,3,3,3,3,3,3,3,3,3,3,3,3,4),(0.,0.0372150073459974,
0.0759036440357819,0.116494755002558,0.15971628635105,0.207036887347821,
0.265275351739583,0.328858620274534,0.377066398240659,0.420570421282261,
0.461281571881092,0.50247045159648,0.542638283169258,0.585163636770142,
0.631190064016801,0.685017456026248,0.763763092019686,0.814055107507527,
0.860541330630645,0.901120921336454,0.940124312769201,0.977290078168108,
1.),.UNSPECIFIED.);
#297=B_SPLINE_CURVE_WITH_KNOTS('',3,(#27116,#27117,#27118,#27119,#27120),
 .UNSPECIFIED.,.F.,.F.,(4,1,4),(1.09621611801068,1.29877304187851,1.50132996574633),
 .UNSPECIFIED.);
#298=B_SPLINE_CURVE_WITH_KNOTS('',3,(#27122,#27123,#27124,#27125),
 .UNSPECIFIED.,.F.,.F.,(4,4),(1.02439235355261,1.09621611801068),
 .UNSPECIFIED.);
#299=B_SPLINE_CURVE_WITH_KNOTS('',3,(#27129,#27130,#27131,#27132),
 .UNSPECIFIED.,.F.,.F.,(4,4),(0.396818713712603,0.466059241584687),
 .UNSPECIFIED.);
#300=B_SPLINE_CURVE_WITH_KNOTS('',3,(#27134,#27135,#27136,#27137,#27138,
#27139,#27140),.UNSPECIFIED.,.F.,.F.,(4,2,1,4),(9.99213751786565E-5,0.127637384843918,
0.289146182165162,0.396818713712658),.UNSPECIFIED.);
#301=B_SPLINE_CURVE_WITH_KNOTS('',3,(#27141,#27142,#27143,#27144,#27145,
#27146,#27147,#27148,#27149,#27150,#27151,#27152,#27153,#27154,#27155,#27156,
#27157,#27158,#27159,#27160,#27161,#27162,#27163,#27164,#27165,#27166,#27167,
#27168,#27169,#27170,#27171,#27172,#27173,#27174,#27175,#27176,#27177,#27178,
#27179,#27180,#27181,#27182,#27183,#27184,#27185,#27186,#27187,#27188,#27189,
#27190,#27191,#27192,#27193,#27194,#27195,#27196,#27197,#27198,#27199,#27200,
#27201,#27202,#27203,#27204,#27205,#27206,#27207),.UNSPECIFIED.,.F.,.F.,
(4,3,3,3,3,3,3,3,3,3,3,3,3,3,3,3,3,3,3,3,3,3,4),(0.,0.0372142743249414,
0.0759021060272706,0.116492303751609,0.15971273797737,0.207031854381263,
0.265265992983546,0.328853755149798,0.37706150936917,0.420565256169277,
0.461276052626863,0.50245372219686,0.542621232263039,0.585145966617605,
0.631171144882026,0.684995344588453,0.76374650844134,0.814042029226479,
0.860531521919859,0.901112266515804,0.94011665297404,0.977283203644708,
1.),.UNSPECIFIED.);
#302=B_SPLINE_CURVE_WITH_KNOTS('',3,(#27220,#27221,#27222,#27223,#27224,
#27225,#27226,#27227,#27228,#27229,#27230,#27231,#27232,#27233,#27234,#27235,
#27236,#27237,#27238,#27239,#27240,#27241,#27242,#27243,#27244,#27245,#27246,
#27247,#27248,#27249,#27250,#27251,#27252,#27253,#27254,#27255,#27256,#27257,
#27258,#27259,#27260,#27261,#27262,#27263,#27264,#27265,#27266,#27267,#27268,
#27269,#27270,#27271,#27272,#27273,#27274,#27275,#27276,#27277,#27278,#27279,
#27280,#27281,#27282,#27283,#27284,#27285,#27286),.UNSPECIFIED.,.F.,.F.,
(4,3,3,3,3,3,3,3,3,3,3,3,3,3,3,3,3,3,3,3,3,3,4),(0.,0.0372150196070085,
0.0759036698970674,0.116494796498611,0.15971634697478,0.207036974548953,
0.265275520854355,0.328858695194123,0.377066470534805,0.420570496312742,
0.461281651387635,0.502470683175898,0.542638526520072,0.585163896376155,
0.631190349090315,0.685017798075316,0.763763348556487,0.814055329762754,
0.860541497322065,0.901121082418717,0.94012446955152,0.977290233255848,
1.),.UNSPECIFIED.);
#303=B_SPLINE_CURVE_WITH_KNOTS('',3,(#27288,#27289,#27290,#27291,#27292,
#27293),.UNSPECIFIED.,.F.,.F.,(4,1,1,4),(1.09363288142463,1.20698114379938,
1.26365527498675,1.49035179973623),.UNSPECIFIED.);
#304=B_SPLINE_CURVE_WITH_KNOTS('',3,(#27295,#27296,#27297,#27298),
 .UNSPECIFIED.,.F.,.F.,(4,4),(1.02439235355261,1.09363288142469),
 .UNSPECIFIED.);
#305=B_SPLINE_CURVE_WITH_KNOTS('',3,(#27302,#27303,#27304,#27305),
 .UNSPECIFIED.,.F.,.F.,(4,4),(0.405213665159311,0.477037429617386),
 .UNSPECIFIED.);
#306=B_SPLINE_CURVE_WITH_KNOTS('',3,(#27307,#27308,#27309,#27310,#27311),
 .UNSPECIFIED.,.F.,.F.,(4,1,4),(0.000100096646392837,0.202656880902853,
0.405213665159313),.UNSPECIFIED.);
#307=B_SPLINE_CURVE_WITH_KNOTS('',3,(#27312,#27313,#27314,#27315,#27316,
#27317,#27318,#27319,#27320,#27321,#27322,#27323,#27324,#27325,#27326,#27327,
#27328,#27329,#27330,#27331,#27332,#27333,#27334,#27335,#27336,#27337,#27338,
#27339,#27340,#27341,#27342,#27343,#27344,#27345,#27346,#27347,#27348,#27349,
#27350,#27351,#27352,#27353,#27354,#27355,#27356,#27357,#27358,#27359,#27360,
#27361,#27362,#27363,#27364,#27365,#27366,#27367,#27368,#27369,#27370,#27371,
#27372,#27373,#27374,#27375,#27376,#27377,#27378),.UNSPECIFIED.,.F.,.F.,
(4,3,3,3,3,3,3,3,3,3,3,3,3,3,3,3,3,3,3,3,3,3,4),(0.,0.0372142122738283,
0.0759019766651123,0.116492099285913,0.159712445400096,0.207031446837133,
0.265265278177762,0.328853304622193,0.377061038248202,0.420564750072856,
0.461275507649365,0.502452205884434,0.542619564376986,0.585144107738491,
0.631169015934125,0.684992668379561,0.763744501284671,0.81404021150862,
0.860530158631465,0.901110881237409,0.94011523948485,0.977281743245876,
1.),.UNSPECIFIED.);
#308=B_SPLINE_CURVE_WITH_KNOTS('',3,(#27420,#27421,#27422,#27423,#27424,
#27425,#27426,#27427,#27428,#27429,#27430,#27431,#27432,#27433,#27434,#27435,
#27436,#27437,#27438,#27439,#27440,#27441,#27442,#27443,#27444,#27445,#27446,
#27447,#27448,#27449,#27450,#27451,#27452,#27453,#27454,#27455,#27456,#27457,
#27458,#27459,#27460,#27461,#27462,#27463,#27464,#27465,#27466,#27467,#27468,
#27469,#27470,#27471,#27472,#27473,#27474,#27475,#27476,#27477,#27478,#27479,
#27480,#27481,#27482,#27483,#27484,#27485,#27486,#27487,#27488,#27489,#27490,
#27491,#27492,#27493,#27494,#27495,#27496,#27497,#27498,#27499,#27500,#27501,
#27502,#27503,#27504,#27505,#27506,#27507,#27508,#27509,#27510,#27511,#27512,
#27513,#27514,#27515,#27516),.UNSPECIFIED.,.F.,.F.,(4,3,3,3,3,3,3,3,3,3,
3,3,3,3,3,3,3,3,3,3,3,3,3,3,3,3,3,3,3,3,3,3,4),(0.,0.0249561576389582,0.0505230689649538,
0.0768014946929841,0.103927702815189,0.132729761515055,0.163050828032849,
0.195526914275497,0.231526666456084,0.275596223262613,0.320871459308699,
0.357021183774404,0.38928558844534,0.419345587098888,0.447888984260675,
0.475288232374118,0.503212894511638,0.530052590323374,0.557847043091744,
0.587565866489206,0.619084976767266,0.653310159114776,0.692899272183232,
0.744530806263077,0.780991793284318,0.81370690045686,0.84424865112698,0.87328209994709,
0.901172514215133,0.927739555510914,0.953706026754902,0.978856478652302,
1.),.UNSPECIFIED.);
#309=B_SPLINE_CURVE_WITH_KNOTS('',3,(#27518,#27519,#27520,#27521),
 .UNSPECIFIED.,.F.,.F.,(4,4),(-1.,0.),.UNSPECIFIED.);
#310=B_SPLINE_CURVE_WITH_KNOTS('',3,(#27522,#27523,#27524,#27525,#27526,
#27527,#27528,#27529,#27530,#27531,#27532,#27533,#27534,#27535,#27536,#27537,
#27538,#27539,#27540,#27541,#27542,#27543,#27544,#27545,#27546,#27547,#27548,
#27549,#27550,#27551,#27552,#27553,#27554,#27555,#27556,#27557,#27558,#27559,
#27560,#27561,#27562,#27563,#27564,#27565,#27566,#27567,#27568,#27569,#27570,
#27571,#27572,#27573,#27574,#27575,#27576,#27577,#27578,#27579,#27580,#27581,
#27582,#27583,#27584,#27585,#27586,#27587,#27588),.UNSPECIFIED.,.F.,.F.,
(4,3,3,3,3,3,3,3,3,3,3,3,3,3,3,3,3,3,3,3,3,3,4),(0.,0.037215019607135,0.0759036698970782,
0.116494796498149,0.159716346974602,0.207036974549224,0.265275520853068,
0.328858695193836,0.377066470534692,0.420570496312419,0.461281651387186,
0.502470683172426,0.542638526516054,0.585163896371612,0.631190349085662,
0.685017798068377,0.763763348551283,0.814055329757142,0.860541497317856,
0.901121082414824,0.940124469547107,0.977290233251386,1.),.UNSPECIFIED.);
#311=B_SPLINE_CURVE_WITH_KNOTS('',3,(#27631,#27632,#27633,#27634,#27635,
#27636,#27637,#27638,#27639,#27640,#27641,#27642,#27643,#27644,#27645,#27646,
#27647,#27648,#27649,#27650,#27651,#27652,#27653,#27654,#27655,#27656,#27657,
#27658,#27659,#27660,#27661,#27662,#27663,#27664,#27665,#27666,#27667,#27668,
#27669,#27670,#27671,#27672,#27673,#27674,#27675,#27676,#27677,#27678,#27679,
#27680,#27681,#27682,#27683,#27684,#27685,#27686,#27687,#27688,#27689,#27690,
#27691,#27692,#27693,#27694,#27695,#27696,#27697),.UNSPECIFIED.,.F.,.F.,
(4,3,3,3,3,3,3,3,3,3,3,3,3,3,3,3,3,3,3,3,3,3,4),(0.,0.0372142121292241,
0.0759019763640333,0.116492098810497,0.159712444720991,0.207031445894069,
0.265265276534927,0.328853303564281,0.377061037137402,0.420564748877918,
0.461275506361833,0.502452202278194,0.542619560431093,0.585144103359907,
0.631169010935895,0.684992662113913,0.763744496585435,0.814040207302302,
0.860530155476726,0.901110878061003,0.940115236269481,0.977281739945585,
1.),.UNSPECIFIED.);
#312=B_SPLINE_CURVE_WITH_KNOTS('',3,(#27699,#27700,#27701,#27702),
 .UNSPECIFIED.,.F.,.F.,(4,4),(0.,1.),.UNSPECIFIED.);
#313=B_SPLINE_CURVE_WITH_KNOTS('',3,(#27704,#27705,#27706,#27707,#27708,
#27709,#27710,#27711,#27712,#27713,#27714,#27715,#27716,#27717,#27718,#27719,
#27720,#27721,#27722,#27723,#27724,#27725,#27726,#27727,#27728,#27729,#27730,
#27731,#27732,#27733,#27734,#27735,#27736,#27737,#27738,#27739,#27740,#27741,
#27742,#27743,#27744,#27745,#27746,#27747,#27748,#27749,#27750,#27751,#27752,
#27753,#27754,#27755,#27756,#27757,#27758,#27759,#27760,#27761,#27762,#27763,
#27764,#27765,#27766,#27767,#27768,#27769,#27770,#27771,#27772,#27773,#27774,
#27775,#27776,#27777,#27778,#27779,#27780,#27781,#27782,#27783,#27784,#27785,
#27786,#27787,#27788,#27789,#27790,#27791,#27792,#27793,#27794,#27795,#27796,
#27797,#27798,#27799,#27800),.UNSPECIFIED.,.F.,.F.,(4,3,3,3,3,3,3,3,3,3,
3,3,3,3,3,3,3,3,3,3,3,3,3,3,3,3,3,3,3,3,3,3,4),(0.,0.0249709672790016,0.0505536024514495,
0.0768489351040166,0.103993630089062,0.132817340140775,0.163164016125442,
0.195672955688052,0.231723181390253,0.276005254460143,0.321254926056384,
0.357363044451917,0.389612545656904,0.419666623911194,0.448208487868328,
0.475608730563432,0.503750970182619,0.530595750607696,0.558398676707341,
0.58813364847834,0.619679816365933,0.653955102605481,0.693711324455342,
0.744658928774623,0.781071741936943,0.813756877135301,0.844275170967022,
0.873288582738427,0.901161117024878,0.927712121392446,0.953663439792987,
0.97879939830999,1.),.UNSPECIFIED.);
#314=B_SPLINE_CURVE_WITH_KNOTS('',3,(#27823,#27824,#27825,#27826,#27827),
 .UNSPECIFIED.,.F.,.F.,(4,1,4),(0.000100096646392838,0.202656880902853,
0.405213665159313),.UNSPECIFIED.);
#315=B_SPLINE_CURVE_WITH_KNOTS('',3,(#27830,#27831,#27832,#27833,#27834),
 .UNSPECIFIED.,.F.,.F.,(4,1,4),(-0.405213665159313,-0.202656880902853,-0.000100096646392838),
 .UNSPECIFIED.);
#316=B_SPLINE_CURVE_WITH_KNOTS('',3,(#27860,#27861,#27862,#27863),
 .UNSPECIFIED.,.F.,.F.,(4,4),(-0.477037429617388,-0.405213665159311),
 .UNSPECIFIED.);
#317=B_SPLINE_CURVE_WITH_KNOTS('',3,(#27864,#27865,#27866,#27867),
 .UNSPECIFIED.,.F.,.F.,(4,4),(0.405213665159311,0.477037429617388),
 .UNSPECIFIED.);
#318=B_SPLINE_CURVE_WITH_KNOTS('',3,(#27901,#27902,#27903,#27904,#27905,
#27906,#27907,#27908),.UNSPECIFIED.,.F.,.F.,(4,2,2,4),(-1.49035179973623,
-1.36281421029337,-1.23517682544946,-1.09363288142463),.UNSPECIFIED.);
#319=B_SPLINE_CURVE_WITH_KNOTS('',3,(#27911,#27912,#27913,#27914,#27915,
#27916,#27917,#27918),.UNSPECIFIED.,.F.,.F.,(4,2,2,4),(1.09363288142463,
1.23517682544946,1.36281421029337,1.49035179973623),.UNSPECIFIED.);
#320=B_SPLINE_CURVE_WITH_KNOTS('',3,(#27935,#27936,#27937,#27938),
 .UNSPECIFIED.,.F.,.F.,(4,4),(-1.09363288142469,-1.02439235355261),
 .UNSPECIFIED.);
#321=B_SPLINE_CURVE_WITH_KNOTS('',3,(#27939,#27940,#27941,#27942),
 .UNSPECIFIED.,.F.,.F.,(4,4),(1.02439235355261,1.09363288142469),
 .UNSPECIFIED.);
#322=B_SPLINE_CURVE_WITH_KNOTS('',3,(#27945,#27946,#27947,#27948,#27949,
#27950,#27951,#27952,#27953,#27954,#27955,#27956,#27957,#27958,#27959,#27960,
#27961,#27962,#27963,#27964,#27965,#27966,#27967,#27968,#27969,#27970,#27971,
#27972,#27973,#27974,#27975,#27976,#27977,#27978,#27979,#27980,#27981,#27982,
#27983,#27984,#27985,#27986,#27987,#27988,#27989,#27990,#27991,#27992,#27993,
#27994,#27995,#27996,#27997,#27998,#27999,#28000,#28001,#28002,#28003,#28004,
#28005,#28006,#28007,#28008,#28009,#28010,#28011,#28012,#28013,#28014,#28015,
#28016,#28017,#28018,#28019,#28020,#28021,#28022,#28023,#28024,#28025,#28026,
#28027,#28028,#28029,#28030,#28031,#28032,#28033,#28034,#28035,#28036,#28037,
#28038,#28039,#28040,#28041),.UNSPECIFIED.,.F.,.F.,(4,3,3,3,3,3,3,3,3,3,
3,3,3,3,3,3,3,3,3,3,3,3,3,3,3,3,3,3,3,3,3,3,4),(0.,0.0249709948250819,0.0505536593533966,
0.0768490236852142,0.10399375345847,0.132817504688352,0.163164229887591,
0.195673233277454,0.231723557259323,0.276005984111853,0.321255610104862,
0.357363640101273,0.389613108945727,0.419667173118957,0.448209031765858,
0.475609274173033,0.503751910718119,0.530596724096154,0.558399690027093,
0.588134716371141,0.619680960018544,0.653956366554597,0.693712941226904,
0.744659534140973,0.781072281842521,0.81375738602271,0.844275660836252,
0.873289059550228,0.901161584288134,0.927712584049702,0.953663898808582,
0.978799857569016,1.),.UNSPECIFIED.);
#323=B_SPLINE_CURVE_WITH_KNOTS('',3,(#28043,#28044,#28045,#28046,#28047,
#28048,#28049),.UNSPECIFIED.,.F.,.F.,(4,1,2,4),(-0.396818713712658,-0.289146182165162,
-0.127637384843918,-9.99213751786565E-5),.UNSPECIFIED.);
#324=B_SPLINE_CURVE_WITH_KNOTS('',3,(#28095,#28096,#28097,#28098,#28099,
#28100,#28101,#28102,#28103,#28104,#28105,#28106,#28107,#28108,#28109,#28110,
#28111,#28112,#28113,#28114,#28115,#28116,#28117,#28118,#28119,#28120,#28121,
#28122,#28123,#28124,#28125,#28126,#28127,#28128,#28129,#28130,#28131,#28132,
#28133,#28134,#28135,#28136,#28137,#28138,#28139,#28140,#28141,#28142,#28143,
#28144,#28145,#28146,#28147,#28148,#28149,#28150,#28151,#28152,#28153,#28154,
#28155,#28156,#28157,#28158,#28159,#28160,#28161,#28162,#28163,#28164,#28165,
#28166,#28167,#28168,#28169,#28170,#28171,#28172,#28173,#28174,#28175,#28176,
#28177,#28178,#28179,#28180,#28181,#28182,#28183,#28184,#28185,#28186,#28187,
#28188,#28189,#28190,#28191),.UNSPECIFIED.,.F.,.F.,(4,3,3,3,3,3,3,3,3,3,
3,3,3,3,3,3,3,3,3,3,3,3,3,3,3,3,3,3,3,3,3,3,4),(0.,0.0249561607551759,0.0505230751945413,
0.0768015040119749,0.103927715157316,0.13272977655757,0.163050845426121,
0.195526933356038,0.231526685629517,0.275596237711758,0.320871472854773,
0.357021212133758,0.389285626160042,0.419345632279732,0.447889035910775,
0.475288289852361,0.503212993519124,0.530052682547603,0.557847129410532,
0.587565949393601,0.619085059687446,0.653310249780398,0.692899411004627,
0.744530685907878,0.780991641273838,0.813706725614835,0.844248457013025,
0.873281888573613,0.90117228690679,0.927739312487755,0.953705768715376,
0.978856204742226,1.),.UNSPECIFIED.);
#325=B_SPLINE_CURVE_WITH_KNOTS('',3,(#28193,#28194,#28195,#28196),
 .UNSPECIFIED.,.F.,.F.,(4,4),(-1.,0.),.UNSPECIFIED.);
#326=B_SPLINE_CURVE_WITH_KNOTS('',3,(#28198,#28199,#28200,#28201,#28202,
#28203,#28204,#28205,#28206,#28207,#28208,#28209,#28210,#28211,#28212,#28213,
#28214,#28215,#28216,#28217,#28218,#28219,#28220,#28221,#28222,#28223,#28224,
#28225,#28226,#28227,#28228,#28229,#28230,#28231,#28232,#28233,#28234,#28235,
#28236,#28237,#28238,#28239,#28240,#28241,#28242,#28243,#28244,#28245,#28246,
#28247,#28248,#28249,#28250,#28251,#28252,#28253,#28254,#28255,#28256,#28257,
#28258,#28259,#28260,#28261,#28262,#28263,#28264),.UNSPECIFIED.,.F.,.F.,
(4,3,3,3,3,3,3,3,3,3,3,3,3,3,3,3,3,3,3,3,3,3,4),(0.,0.0372150073460308,
0.075903644036051,0.116494755002737,0.159716286351032,0.207036887346632,
0.265275351737657,0.328858620272782,0.377066398239113,0.420570421280702,
0.461281571879719,0.502470451594025,0.542638283166554,0.585163636766946,
0.631190064013865,0.685017456021953,0.763763092016465,0.814055107505727,
0.860541330629295,0.901120921335073,0.94012431276777,0.977290078166758,
1.),.UNSPECIFIED.);
#327=B_SPLINE_CURVE_WITH_KNOTS('',3,(#28308,#28309,#28310,#28311,#28312,
#28313,#28314,#28315,#28316,#28317,#28318,#28319,#28320,#28321,#28322,#28323,
#28324,#28325,#28326,#28327,#28328,#28329,#28330,#28331,#28332,#28333,#28334,
#28335,#28336,#28337,#28338,#28339,#28340,#28341,#28342,#28343,#28344,#28345,
#28346,#28347,#28348,#28349,#28350,#28351,#28352,#28353,#28354,#28355,#28356,
#28357,#28358,#28359,#28360,#28361,#28362,#28363,#28364,#28365,#28366,#28367,
#28368,#28369,#28370,#28371,#28372,#28373,#28374),.UNSPECIFIED.,.F.,.F.,
(4,3,3,3,3,3,3,3,3,3,3,3,3,3,3,3,3,3,3,3,3,3,4),(0.,0.0372142743247427,
0.0759021060270489,0.116492303751548,0.15971273797765,0.207031854381748,
0.26526599298503,0.328853755151349,0.377061509370842,0.420565256170683,
0.461276052627892,0.502453722200266,0.542621232267039,0.585145966622121,
0.631171144887316,0.684995344592088,0.763746508444066,0.814042029230295,
0.860531521922721,0.901112266518215,0.940116652976414,0.977283203647236,
1.),.UNSPECIFIED.);
#328=B_SPLINE_CURVE_WITH_KNOTS('',3,(#28376,#28377,#28378,#28379),
 .UNSPECIFIED.,.F.,.F.,(4,4),(0.,1.),.UNSPECIFIED.);
#329=B_SPLINE_CURVE_WITH_KNOTS('',3,(#28381,#28382,#28383,#28384,#28385,
#28386,#28387,#28388,#28389,#28390,#28391,#28392,#28393,#28394,#28395,#28396,
#28397,#28398,#28399,#28400,#28401,#28402,#28403,#28404,#28405,#28406,#28407,
#28408,#28409,#28410,#28411,#28412,#28413,#28414,#28415,#28416,#28417,#28418,
#28419,#28420,#28421,#28422,#28423,#28424,#28425,#28426,#28427,#28428,#28429,
#28430,#28431,#28432,#28433,#28434,#28435,#28436,#28437,#28438,#28439,#28440,
#28441,#28442,#28443,#28444,#28445,#28446,#28447,#28448,#28449,#28450,#28451,
#28452,#28453,#28454,#28455,#28456,#28457,#28458,#28459,#28460,#28461,#28462,
#28463,#28464,#28465,#28466,#28467,#28468,#28469,#28470,#28471,#28472,#28473,
#28474,#28475,#28476,#28477),.UNSPECIFIED.,.F.,.F.,(4,3,3,3,3,3,3,3,3,3,
3,3,3,3,3,3,3,3,3,3,3,3,3,3,3,3,3,3,3,3,3,3,4),(0.,0.024970994825275,0.0505536593526047,
0.0768490236835355,0.103993753457102,0.132817504687059,0.163164229886278,
0.195673233276151,0.231723557257424,0.27600598410841,0.321255610101634,
0.357363640098368,0.389613108942904,0.419667173116849,0.448209031763796,
0.475609274170904,0.503751910715254,0.5305967240942,0.558399690026767,0.588134716370664,
0.619680960018106,0.653956366554247,0.69371294122632,0.744659534141732,
0.781072281843131,0.813757386023587,0.844275660837523,0.873289059551439,
0.901161584289068,0.927712584050538,0.953663898809603,0.978799857570089,
1.),.UNSPECIFIED.);
#330=B_SPLINE_CURVE_WITH_KNOTS('',3,(#28512,#28513,#28514,#28515,#28516,
#28517,#28518,#28519),.UNSPECIFIED.,.F.,.F.,(4,2,2,4),(9.99213751786348E-5,
0.127637384843918,0.255274769687837,0.396818713712658),.UNSPECIFIED.);
#331=B_SPLINE_CURVE_WITH_KNOTS('',3,(#28522,#28523,#28524,#28525,#28526,
#28527,#28528,#28529),.UNSPECIFIED.,.F.,.F.,(4,2,2,4),(-0.396818713712658,
-0.255274769687837,-0.127637384843918,-9.99213751786348E-5),
 .UNSPECIFIED.);
#332=B_SPLINE_CURVE_WITH_KNOTS('',3,(#28555,#28556,#28557,#28558),
 .UNSPECIFIED.,.F.,.F.,(4,4),(-0.466059241584687,-0.396818713712602),
 .UNSPECIFIED.);
#333=B_SPLINE_CURVE_WITH_KNOTS('',3,(#28559,#28560,#28561,#28562),
 .UNSPECIFIED.,.F.,.F.,(4,4),(0.396818713712602,0.466059241584687),
 .UNSPECIFIED.);
#334=B_SPLINE_CURVE_WITH_KNOTS('',3,(#28584,#28585,#28586,#28587,#28588),
 .UNSPECIFIED.,.F.,.F.,(4,1,4),(-1.50125809047561,-1.29870116660779,-1.09614424273996),
 .UNSPECIFIED.);
#335=B_SPLINE_CURVE_WITH_KNOTS('',3,(#28591,#28592,#28593,#28594,#28595),
 .UNSPECIFIED.,.F.,.F.,(4,1,4),(1.09614424273996,1.29870116660779,1.50125809047561),
 .UNSPECIFIED.);
#336=B_SPLINE_CURVE_WITH_KNOTS('',3,(#28612,#28613,#28614,#28615),
 .UNSPECIFIED.,.F.,.F.,(4,4),(-1.09614424273996,-1.02432047828189),
 .UNSPECIFIED.);
#337=B_SPLINE_CURVE_WITH_KNOTS('',3,(#28616,#28617,#28618,#28619),
 .UNSPECIFIED.,.F.,.F.,(4,4),(1.02432047828189,1.09614424273996),
 .UNSPECIFIED.);
#338=B_SPLINE_CURVE_WITH_KNOTS('',3,(#28668,#28669,#28670,#28671),
 .UNSPECIFIED.,.F.,.F.,(4,4),(-0.466059241584687,-0.396818713712603),
 .UNSPECIFIED.);
#339=B_SPLINE_CURVE_WITH_KNOTS('',3,(#28675,#28676,#28677,#28678),
 .UNSPECIFIED.,.F.,.F.,(4,4),(-1.09621611801068,-1.02439235355261),
 .UNSPECIFIED.);
#340=B_SPLINE_CURVE_WITH_KNOTS('',3,(#28682,#28683,#28684,#28685),
 .UNSPECIFIED.,.F.,.F.,(4,4),(-0.477037429617386,-0.405213665159311),
 .UNSPECIFIED.);
#341=B_SPLINE_CURVE_WITH_KNOTS('',3,(#28689,#28690,#28691,#28692),
 .UNSPECIFIED.,.F.,.F.,(4,4),(-1.09363288142469,-1.02439235355261),
 .UNSPECIFIED.);
#342=B_SPLINE_CURVE_WITH_KNOTS('',3,(#28735,#28736,#28737,#28738,#28739,
#28740,#28741,#28742,#28743,#28744,#28745,#28746,#28747,#28748,#28749,#28750,
#28751,#28752,#28753,#28754,#28755,#28756,#28757,#28758,#28759,#28760,#28761,
#28762,#28763,#28764,#28765,#28766,#28767,#28768,#28769,#28770,#28771,#28772,
#28773,#28774,#28775,#28776,#28777,#28778,#28779,#28780,#28781,#28782,#28783,
#28784,#28785,#28786,#28787,#28788,#28789,#28790,#28791,#28792,#28793,#28794,
#28795,#28796,#28797,#28798,#28799,#28800,#28801,#28802,#28803,#28804,#28805,
#28806,#28807,#28808,#28809,#28810,#28811,#28812,#28813,#28814,#28815,#28816,
#28817,#28818,#28819,#28820,#28821,#28822,#28823,#28824,#28825,#28826,#28827,
#28828,#28829,#28830,#28831),.UNSPECIFIED.,.F.,.F.,(4,3,3,3,3,3,3,3,3,3,
3,3,3,3,3,3,3,3,3,3,3,3,3,3,3,3,3,3,3,3,3,3,4),(0.,0.0249561607552664,0.0505230751945348,
0.0768015040119973,0.103927715157151,0.132729776557401,0.163050845425953,
0.195526933355796,0.231526685628984,0.275596237711111,0.320871472854167,
0.357021212132904,0.389285626159344,0.419345632279235,0.447889035910456,
0.475288289851987,0.503212993518741,0.530052682547321,0.557847129410434,
0.587565949393458,0.619085059687253,0.653310249780217,0.69289941100446,
0.744530685907743,0.780991641273769,0.813706725614636,0.844248457012843,
0.873281888573462,0.901172286906684,0.927739312487747,0.95370576871536,
0.978856204742182,1.),.UNSPECIFIED.);
#343=B_SPLINE_CURVE_WITH_KNOTS('',3,(#28832,#28833,#28834,#28835),
 .UNSPECIFIED.,.F.,.F.,(4,4),(-1.,0.),.UNSPECIFIED.);
#344=B_SPLINE_CURVE_WITH_KNOTS('',3,(#28876,#28877,#28878,#28879),
 .UNSPECIFIED.,.F.,.F.,(4,4),(0.,1.),.UNSPECIFIED.);
#345=B_SPLINE_CURVE_WITH_KNOTS('',3,(#28948,#28949,#28950,#28951,#28952),
 .UNSPECIFIED.,.F.,.F.,(4,1,4),(-1.50132996574633,-1.29877304187851,-1.09621611801068),
 .UNSPECIFIED.);
#346=B_SPLINE_CURVE_WITH_KNOTS('',3,(#28972,#28973,#28974,#28975,#28976,
#28977,#28978,#28979,#28980,#28981,#28982,#28983,#28984,#28985,#28986,#28987,
#28988,#28989,#28990,#28991,#28992,#28993,#28994,#28995,#28996,#28997,#28998,
#28999,#29000,#29001,#29002,#29003,#29004,#29005,#29006,#29007,#29008,#29009,
#29010,#29011,#29012,#29013,#29014,#29015,#29016,#29017,#29018,#29019,#29020,
#29021,#29022,#29023,#29024,#29025,#29026,#29027,#29028,#29029,#29030,#29031,
#29032,#29033,#29034,#29035,#29036,#29037,#29038,#29039,#29040,#29041,#29042,
#29043,#29044,#29045,#29046,#29047,#29048,#29049,#29050,#29051,#29052,#29053,
#29054,#29055,#29056,#29057,#29058,#29059,#29060,#29061,#29062,#29063,#29064,
#29065,#29066,#29067,#29068),.UNSPECIFIED.,.F.,.F.,(4,3,3,3,3,3,3,3,3,3,
3,3,3,3,3,3,3,3,3,3,3,3,3,3,3,3,3,3,3,3,3,3,4),(0.,0.0249709672484359,0.0505536023890231,
0.076848935008454,0.103993629960391,0.132817339975555,0.163164015919887,
0.195672955438129,0.231723181102756,0.276005254951893,0.321254926517399,
0.357363044848955,0.389612545990367,0.419666624190472,0.448208488100715,
0.475608730754226,0.503750970445978,0.530595750852095,0.558398676932134,
0.588133648681033,0.619679816541673,0.653955102740443,0.693711324443674,
0.744658928150356,0.781071741349566,0.813756876560073,0.844275170394233,
0.873288582162991,0.90116111644343,0.927712120800645,0.953663439191003,
0.978799397693063,1.),.UNSPECIFIED.);
#347=B_SPLINE_CURVE_WITH_KNOTS('',3,(#29069,#29070,#29071,#29072,#29073),
 .UNSPECIFIED.,.F.,.F.,(4,1,4),(-0.405213665159313,-0.202656880902853,-0.000100096646392837),
 .UNSPECIFIED.);
#348=B_SPLINE_CURVE_WITH_KNOTS('',3,(#29116,#29117,#29118,#29119,#29120,
#29121,#29122,#29123,#29124,#29125,#29126,#29127,#29128,#29129,#29130,#29131,
#29132,#29133,#29134,#29135,#29136,#29137,#29138,#29139,#29140,#29141,#29142,
#29143,#29144,#29145,#29146,#29147,#29148,#29149,#29150,#29151,#29152,#29153,
#29154,#29155,#29156,#29157,#29158,#29159,#29160,#29161,#29162,#29163,#29164,
#29165,#29166,#29167,#29168,#29169,#29170,#29171,#29172,#29173,#29174,#29175,
#29176,#29177,#29178,#29179,#29180,#29181,#29182,#29183,#29184,#29185,#29186,
#29187,#29188,#29189,#29190,#29191,#29192,#29193,#29194,#29195,#29196,#29197,
#29198,#29199,#29200,#29201,#29202,#29203,#29204,#29205,#29206,#29207,#29208,
#29209,#29210,#29211,#29212),.UNSPECIFIED.,.F.,.F.,(4,3,3,3,3,3,3,3,3,3,
3,3,3,3,3,3,3,3,3,3,3,3,3,3,3,3,3,3,3,3,3,3,4),(0.,0.0249561576390629,0.0505230689649775,
0.0768014946930641,0.103927702815194,0.132729761515069,0.163050828032914,
0.195526914275558,0.231526666455973,0.275596223262652,0.320871459308736,
0.357021183774344,0.38928558844556,0.419345587099029,0.447888984260831,
0.475288232374163,0.503212894511872,0.530052590323447,0.557847043091724,
0.587565866489155,0.619084976767197,0.653310159114852,0.692899272183628,
0.744530806262874,0.780991793284097,0.813706900456684,0.844248651126759,
0.873282099946833,0.901172514214929,0.927739555510682,0.953706026754719,
0.9788564786521,1.),.UNSPECIFIED.);
#349=B_SPLINE_CURVE_WITH_KNOTS('',3,(#29213,#29214,#29215,#29216),
 .UNSPECIFIED.,.F.,.F.,(4,4),(-1.,0.),.UNSPECIFIED.);
#350=B_SPLINE_CURVE_WITH_KNOTS('',3,(#29258,#29259,#29260,#29261),
 .UNSPECIFIED.,.F.,.F.,(4,4),(0.,1.),.UNSPECIFIED.);
#351=B_SPLINE_CURVE_WITH_KNOTS('',3,(#29326,#29327,#29328,#29329,#29330,
#29331),.UNSPECIFIED.,.F.,.F.,(4,1,1,4),(-1.49035179973623,-1.26365527498675,
-1.20698114379938,-1.09363288142463),.UNSPECIFIED.);
#352=B_SPLINE_CURVE_WITH_KNOTS('',3,(#29537,#29538,#29539,#29540,#29541,
#29542,#29543,#29544,#29545,#29546,#29547,#29548,#29549,#29550,#29551,#29552,
#29553,#29554,#29555,#29556,#29557,#29558,#29559,#29560,#29561,#29562,#29563,
#29564,#29565,#29566,#29567,#29568,#29569,#29570,#29571,#29572,#29573,#29574,
#29575,#29576,#29577,#29578,#29579,#29580,#29581,#29582,#29583,#29584,#29585,
#29586,#29587,#29588,#29589,#29590,#29591,#29592,#29593,#29594,#29595,#29596,
#29597,#29598,#29599,#29600,#29601,#29602,#29603,#29604,#29605,#29606,#29607,
#29608,#29609,#29610,#29611,#29612,#29613,#29614,#29615,#29616,#29617,#29618,
#29619,#29620,#29621,#29622,#29623,#29624,#29625,#29626,#29627,#29628,#29629,
#29630),.UNSPECIFIED.,.F.,.F.,(4,3,3,3,3,3,3,3,3,3,3,3,3,3,3,3,3,3,3,3,
3,3,3,3,3,3,3,3,3,3,3,4),(0.,0.0258707374451698,0.0523995842804884,0.0797001065242145,
0.108495122701971,0.138579548146388,0.170391094738405,0.204740918376836,
0.243564930469247,0.301738535677522,0.342786820776585,0.377562328700043,
0.409462754742929,0.439523776912731,0.468248829463879,0.497342034867759,
0.525270549115699,0.554941139795967,0.585586421921526,0.618112000252219,
0.653483627180876,0.694829905002005,0.747358415243329,0.784774064435163,
0.818382572828511,0.849773402002612,0.879622020764925,0.909716515573693,
0.937043932385008,0.963754510580494,0.989696242215803,1.),.UNSPECIFIED.);
#353=B_SPLINE_CURVE_WITH_KNOTS('',3,(#29632,#29633,#29634,#29635),
 .UNSPECIFIED.,.F.,.F.,(4,4),(-1.,0.),.UNSPECIFIED.);
#354=B_SPLINE_CURVE_WITH_KNOTS('',3,(#29637,#29638,#29639,#29640,#29641,
#29642,#29643,#29644,#29645,#29646,#29647,#29648,#29649,#29650,#29651,#29652,
#29653,#29654,#29655,#29656,#29657,#29658,#29659,#29660,#29661,#29662,#29663,
#29664,#29665,#29666,#29667,#29668,#29669,#29670,#29671,#29672,#29673,#29674,
#29675,#29676,#29677,#29678,#29679,#29680,#29681,#29682,#29683,#29684,#29685,
#29686,#29687,#29688,#29689,#29690,#29691,#29692,#29693,#29694,#29695,#29696,
#29697,#29698,#29699,#29700,#29701,#29702,#29703,#29704,#29705,#29706),
 .UNSPECIFIED.,.F.,.F.,(4,3,3,3,3,3,3,3,3,3,3,3,3,3,3,3,3,3,3,3,3,3,3,4),
(0.,0.0359057501184,0.0731782994099124,0.112196676257152,0.153588188584124,
0.19856311186321,0.251379995782812,0.322351118570897,0.369695903527712,
0.412227930465316,0.451958538122157,0.49032799292638,0.52995524039796,0.570194128050318,
0.613255077113093,0.66118815818441,0.72826108783719,0.783703920872222,0.829758018851651,
0.872318514138739,0.910997179683127,0.94830001070203,0.984014129742057,
1.),.UNSPECIFIED.);
#355=B_SPLINE_CURVE_WITH_KNOTS('',3,(#29742,#29743,#29744,#29745,#29746,
#29747,#29748,#29749,#29750,#29751,#29752,#29753,#29754,#29755,#29756,#29757,
#29758,#29759,#29760,#29761,#29762,#29763,#29764,#29765,#29766,#29767,#29768,
#29769,#29770,#29771,#29772,#29773,#29774,#29775,#29776,#29777,#29778,#29779,
#29780,#29781,#29782,#29783,#29784,#29785,#29786,#29787,#29788,#29789,#29790,
#29791,#29792,#29793,#29794,#29795,#29796,#29797,#29798,#29799,#29800,#29801,
#29802,#29803,#29804,#29805,#29806,#29807,#29808,#29809,#29810,#29811),
 .UNSPECIFIED.,.F.,.F.,(4,3,3,3,3,3,3,3,3,3,3,3,3,3,3,3,3,3,3,3,3,3,3,4),
(0.,0.0359049134463849,0.073176547549646,0.112193893168169,0.153584182812285,
0.198557501853783,0.251370838267118,0.322351741442161,0.369695708180622,
0.412227003870618,0.451956929703973,0.490325803323821,0.529954284988624,
0.570193684366073,0.613255163900098,0.661188823039329,0.728261735081395,
0.783705956052361,0.829760865743545,0.872320649307659,0.91099999721276,
0.948303461797003,0.984018202039666,1.),.UNSPECIFIED.);
#356=B_SPLINE_CURVE_WITH_KNOTS('',3,(#29813,#29814,#29815,#29816),
 .UNSPECIFIED.,.F.,.F.,(4,4),(0.,1.),.UNSPECIFIED.);
#357=B_SPLINE_CURVE_WITH_KNOTS('',3,(#29818,#29819,#29820,#29821,#29822,
#29823,#29824,#29825,#29826,#29827,#29828,#29829,#29830,#29831,#29832,#29833,
#29834,#29835,#29836,#29837,#29838,#29839,#29840,#29841,#29842,#29843,#29844,
#29845,#29846,#29847,#29848,#29849,#29850,#29851,#29852,#29853,#29854,#29855,
#29856,#29857,#29858,#29859,#29860,#29861,#29862,#29863,#29864,#29865,#29866,
#29867,#29868,#29869,#29870,#29871,#29872,#29873,#29874,#29875,#29876,#29877,
#29878,#29879,#29880,#29881,#29882,#29883,#29884,#29885,#29886,#29887,#29888,
#29889,#29890,#29891,#29892,#29893,#29894,#29895,#29896,#29897,#29898,#29899,
#29900,#29901,#29902,#29903,#29904,#29905,#29906,#29907,#29908,#29909,#29910,
#29911),.UNSPECIFIED.,.F.,.F.,(4,3,3,3,3,3,3,3,3,3,3,3,3,3,3,3,3,3,3,3,
3,3,3,3,3,3,3,3,3,3,3,4),(0.,0.0258806755131893,0.0524200922167716,0.0797320051430074,
0.108539985769749,0.138639209785132,0.170468542508365,0.204841962640731,
0.243705620941324,0.301747786726151,0.342801252332619,0.377583664170473,
0.409491204995713,0.439559328397146,0.468291405426299,0.497246492955408,
0.525185050106943,0.554860984475259,0.585493446299901,0.618003829089383,
0.653355383451557,0.694654043666211,0.747235195717053,0.784647728535492,
0.818250751836891,0.849635399921593,0.879477588119271,0.909608191089453,
0.936927404966159,0.963630037681853,0.989563296559285,1.),.UNSPECIFIED.);
#358=B_SPLINE_CURVE_WITH_KNOTS('',3,(#29934,#29935,#29936,#29937,#29938),
 .UNSPECIFIED.,.F.,.F.,(4,1,4),(0.000100085581199305,0.2925237931603,0.511841573844625),
 .UNSPECIFIED.);
#359=B_SPLINE_CURVE_WITH_KNOTS('',3,(#29941,#29942,#29943,#29944,#29945),
 .UNSPECIFIED.,.F.,.F.,(4,1,4),(-0.511841573844625,-0.2925237931603,-0.000100085581199305),
 .UNSPECIFIED.);
#360=B_SPLINE_CURVE_WITH_KNOTS('',3,(#29971,#29972,#29973,#29974),
 .UNSPECIFIED.,.F.,.F.,(4,4),(-0.568951195767079,-0.511841573844535),
 .UNSPECIFIED.);
#361=B_SPLINE_CURVE_WITH_KNOTS('',3,(#29975,#29976,#29977,#29978),
 .UNSPECIFIED.,.F.,.F.,(4,4),(0.511841573844535,0.568951195767079),
 .UNSPECIFIED.);
#362=B_SPLINE_CURVE_WITH_KNOTS('',3,(#30000,#30001,#30002,#30003,#30004),
 .UNSPECIFIED.,.F.,.F.,(4,1,4),(-1.80301165508774,-1.58369377785584,-1.29126994154665),
 .UNSPECIFIED.);
#363=B_SPLINE_CURVE_WITH_KNOTS('',3,(#30007,#30008,#30009,#30010,#30011),
 .UNSPECIFIED.,.F.,.F.,(4,1,4),(1.29126994154665,1.58369377785584,1.80301165508774),
 .UNSPECIFIED.);
#364=B_SPLINE_CURVE_WITH_KNOTS('',3,(#30028,#30029,#30030,#30031),
 .UNSPECIFIED.,.F.,.F.,(4,4),(-1.29126994154674,-1.2341603196242),
 .UNSPECIFIED.);
#365=B_SPLINE_CURVE_WITH_KNOTS('',3,(#30032,#30033,#30034,#30035),
 .UNSPECIFIED.,.F.,.F.,(4,4),(1.2341603196242,1.29126994154674),
 .UNSPECIFIED.);
#366=B_SPLINE_CURVE_WITH_KNOTS('',3,(#30040,#30041,#30042,#30043,#30044,
#30045,#30046,#30047,#30048,#30049,#30050,#30051,#30052,#30053,#30054,#30055,
#30056,#30057,#30058,#30059,#30060,#30061,#30062,#30063,#30064,#30065,#30066,
#30067,#30068,#30069,#30070,#30071,#30072,#30073,#30074,#30075,#30076,#30077,
#30078,#30079,#30080,#30081,#30082,#30083,#30084,#30085,#30086,#30087,#30088,
#30089,#30090,#30091,#30092,#30093,#30094,#30095,#30096,#30097,#30098,#30099,
#30100,#30101,#30102,#30103,#30104,#30105,#30106,#30107,#30108,#30109,#30110,
#30111,#30112,#30113,#30114,#30115,#30116,#30117,#30118,#30119,#30120,#30121,
#30122,#30123,#30124,#30125,#30126,#30127,#30128,#30129,#30130,#30131,#30132,
#30133),.UNSPECIFIED.,.F.,.F.,(4,3,3,3,3,3,3,3,3,3,3,3,3,3,3,3,3,3,3,3,
3,3,3,3,3,3,3,3,3,3,3,4),(0.,0.0258806755478976,0.0524200922876265,0.0797320052517776,
0.108539985919231,0.138639209979136,0.170468542753168,0.204841962945636,
0.243705621312987,0.301747784910779,0.34280125092102,0.377583662940723,
0.409491203889412,0.439559327385709,0.468291404493187,0.49724649358827,
0.525185050645796,0.554860984980434,0.585493446871105,0.61800382974593,
0.653355384235859,0.694654044834357,0.747235196465702,0.78464772923462,
0.818250752522057,0.849635400605874,0.879477588809083,0.909608191606812,
0.936927405502566,0.963630038237505,0.989563297137722,1.),.UNSPECIFIED.);
#367=B_SPLINE_CURVE_WITH_KNOTS('',3,(#30135,#30136,#30137,#30138,#30139),
 .UNSPECIFIED.,.F.,.F.,(4,1,4),(-0.511841573844626,-0.2925237931603,-0.000100085581199306),
 .UNSPECIFIED.);
#368=B_SPLINE_CURVE_WITH_KNOTS('',3,(#30195,#30196,#30197,#30198,#30199,
#30200,#30201,#30202,#30203,#30204,#30205,#30206,#30207,#30208,#30209,#30210,
#30211,#30212,#30213,#30214,#30215,#30216,#30217,#30218,#30219,#30220,#30221,
#30222,#30223,#30224,#30225,#30226,#30227,#30228,#30229,#30230,#30231,#30232,
#30233,#30234,#30235,#30236,#30237,#30238,#30239,#30240,#30241,#30242,#30243,
#30244,#30245,#30246,#30247,#30248,#30249,#30250,#30251,#30252,#30253,#30254,
#30255,#30256,#30257,#30258,#30259,#30260,#30261,#30262,#30263,#30264,#30265,
#30266,#30267,#30268,#30269,#30270,#30271,#30272,#30273,#30274,#30275,#30276,
#30277,#30278,#30279,#30280,#30281,#30282,#30283,#30284,#30285,#30286,#30287,
#30288),.UNSPECIFIED.,.F.,.F.,(4,3,3,3,3,3,3,3,3,3,3,3,3,3,3,3,3,3,3,3,
3,3,3,3,3,3,3,3,3,3,3,4),(0.,0.0258707373852982,0.0523995841574412,0.0797001063343714,
0.108495122436769,0.138579547796529,0.170391094289058,0.204740917798661,
0.243564929672972,0.301738533531649,0.342786818919582,0.377562326926431,
0.409462753002346,0.439523775182168,0.468248827730827,0.497342036568372,
0.525270550411946,0.554941141011199,0.585586423119629,0.618112001453677,
0.653483628442009,0.694829906775482,0.747358417163163,0.784774066048828,
0.818382574240286,0.849773403259427,0.87962202189283,0.909716516419622,
0.937043933139065,0.963754511246871,0.989696242803908,1.),.UNSPECIFIED.);
#369=B_SPLINE_CURVE_WITH_KNOTS('',3,(#30290,#30291,#30292,#30293),
 .UNSPECIFIED.,.F.,.F.,(4,4),(-1.,0.),.UNSPECIFIED.);
#370=B_SPLINE_CURVE_WITH_KNOTS('',3,(#30295,#30296,#30297,#30298,#30299,
#30300,#30301,#30302,#30303,#30304,#30305,#30306,#30307,#30308,#30309,#30310,
#30311,#30312,#30313,#30314,#30315,#30316,#30317,#30318,#30319,#30320,#30321,
#30322,#30323,#30324,#30325,#30326,#30327,#30328,#30329,#30330,#30331,#30332,
#30333,#30334,#30335,#30336,#30337,#30338,#30339,#30340,#30341,#30342,#30343,
#30344,#30345,#30346,#30347,#30348,#30349,#30350,#30351,#30352,#30353,#30354,
#30355,#30356,#30357,#30358,#30359,#30360,#30361,#30362,#30363,#30364),
 .UNSPECIFIED.,.F.,.F.,(4,3,3,3,3,3,3,3,3,3,3,3,3,3,3,3,3,3,3,3,3,3,3,4),
(0.,0.0359057503974645,0.0731782999903264,0.112196677171334,0.153588189884582,
0.198563113652405,0.251379998572626,0.322351119089413,0.369695904344816,
0.412227931549056,0.45195853945437,0.490327994460789,0.529955241857638,
0.570194129909524,0.613255079462038,0.661188161329761,0.728261095682754,
0.783703926991951,0.829758024663586,0.872318518497689,0.910997184172885,
0.948300015335705,0.984014134572557,1.),.UNSPECIFIED.);
#371=B_SPLINE_CURVE_WITH_KNOTS('',3,(#30399,#30400,#30401,#30402,#30403,
#30404,#30405,#30406,#30407,#30408,#30409,#30410,#30411,#30412,#30413,#30414,
#30415,#30416,#30417,#30418,#30419,#30420,#30421,#30422,#30423,#30424,#30425,
#30426,#30427,#30428,#30429,#30430,#30431,#30432,#30433,#30434,#30435,#30436,
#30437,#30438,#30439,#30440,#30441,#30442,#30443,#30444,#30445,#30446,#30447,
#30448,#30449,#30450,#30451,#30452,#30453,#30454,#30455,#30456,#30457,#30458,
#30459,#30460,#30461,#30462,#30463,#30464,#30465,#30466,#30467,#30468),
 .UNSPECIFIED.,.F.,.F.,(4,3,3,3,3,3,3,3,3,3,3,3,3,3,3,3,3,3,3,3,3,3,3,4),
(0.,0.0359049133077996,0.0731765472614101,0.112193892714089,0.153584182166311,
0.198557500964563,0.251370836880033,0.322351741174105,0.369695707765568,
0.412227003323922,0.451956929034388,0.490325802554425,0.529954284258119,
0.5701936834371,0.613255162727241,0.661188821470719,0.728261731182501,0.783705953011855,
0.829760862856234,0.872320647142176,0.910999994982448,0.948303459495199,
0.984018199640234,1.),.UNSPECIFIED.);
#372=B_SPLINE_CURVE_WITH_KNOTS('',3,(#30469,#30470,#30471,#30472),
 .UNSPECIFIED.,.F.,.F.,(4,4),(0.,1.),.UNSPECIFIED.);
#373=B_SPLINE_CURVE_WITH_KNOTS('',3,(#30494,#30495,#30496,#30497,#30498),
 .UNSPECIFIED.,.F.,.F.,(4,1,4),(0.000100085581199306,0.2925237931603,0.511841573844626),
 .UNSPECIFIED.);
#374=B_SPLINE_CURVE_WITH_KNOTS('',3,(#30525,#30526,#30527,#30528),
 .UNSPECIFIED.,.F.,.F.,(4,4),(-0.568951195767079,-0.511841573844535),
 .UNSPECIFIED.);
#375=B_SPLINE_CURVE_WITH_KNOTS('',3,(#30529,#30530,#30531,#30532),
 .UNSPECIFIED.,.F.,.F.,(4,4),(0.511841573844535,0.568951195767079),
 .UNSPECIFIED.);
#376=B_SPLINE_CURVE_WITH_KNOTS('',3,(#30554,#30555,#30556,#30557,#30558),
 .UNSPECIFIED.,.F.,.F.,(4,1,4),(-1.82014070277373,-1.52771686646454,-1.30839898923264),
 .UNSPECIFIED.);
#377=B_SPLINE_CURVE_WITH_KNOTS('',3,(#30561,#30562,#30563,#30564,#30565),
 .UNSPECIFIED.,.F.,.F.,(4,1,4),(1.30839898923264,1.52771686646454,1.82014070277373),
 .UNSPECIFIED.);
#378=B_SPLINE_CURVE_WITH_KNOTS('',3,(#30582,#30583,#30584,#30585),
 .UNSPECIFIED.,.F.,.F.,(4,4),(-1.30839898923273,-1.25128936731019),
 .UNSPECIFIED.);
#379=B_SPLINE_CURVE_WITH_KNOTS('',3,(#30586,#30587,#30588,#30589),
 .UNSPECIFIED.,.F.,.F.,(4,4),(1.25128936731019,1.30839898923273),
 .UNSPECIFIED.);
#380=B_SPLINE_CURVE_WITH_KNOTS('',3,(#30594,#30595,#30596,#30597),
 .UNSPECIFIED.,.F.,.F.,(4,4),(-0.568951195767077,-0.511841573844537),
 .UNSPECIFIED.);
#381=B_SPLINE_CURVE_WITH_KNOTS('',3,(#30601,#30602,#30603,#30604),
 .UNSPECIFIED.,.F.,.F.,(4,4),(-1.30839898923273,-1.25128936731019),
 .UNSPECIFIED.);
#382=B_SPLINE_CURVE_WITH_KNOTS('',3,(#30608,#30609,#30610,#30611),
 .UNSPECIFIED.,.F.,.F.,(4,4),(-0.568951195767079,-0.511841573844536),
 .UNSPECIFIED.);
#383=B_SPLINE_CURVE_WITH_KNOTS('',3,(#30615,#30616,#30617,#30618),
 .UNSPECIFIED.,.F.,.F.,(4,4),(-1.29126994154674,-1.2341603196242),
 .UNSPECIFIED.);
#384=B_SPLINE_CURVE_WITH_KNOTS('',3,(#30679,#30680,#30681,#30682,#30683,
#30684,#30685,#30686,#30687,#30688,#30689,#30690,#30691,#30692,#30693,#30694,
#30695,#30696,#30697,#30698,#30699,#30700,#30701,#30702,#30703,#30704,#30705,
#30706,#30707,#30708,#30709,#30710,#30711,#30712,#30713,#30714,#30715,#30716,
#30717,#30718,#30719,#30720,#30721,#30722,#30723,#30724,#30725,#30726,#30727,
#30728,#30729,#30730,#30731,#30732,#30733,#30734,#30735,#30736,#30737,#30738,
#30739,#30740,#30741,#30742,#30743,#30744,#30745,#30746,#30747,#30748),
 .UNSPECIFIED.,.F.,.F.,(4,3,3,3,3,3,3,3,3,3,3,3,3,3,3,3,3,3,3,3,3,3,3,4),
(0.,0.0359057503975373,0.0731782999904773,0.112196677171571,0.153588189884912,
0.198563113652762,0.251379998573341,0.322351119089333,0.36969590434482,
0.412227931549108,0.451958539454481,0.490327994460949,0.529955241857821,
0.570194129909769,0.613255079462367,0.66118816133035,0.728261095684453,
0.783703926993341,0.829758024664918,0.872318518498689,0.910997184173894,
0.948300015336798,0.98401413457368,1.),.UNSPECIFIED.);
#385=B_SPLINE_CURVE_WITH_KNOTS('',3,(#30750,#30751,#30752,#30753,#30754),
 .UNSPECIFIED.,.F.,.F.,(4,1,4),(1.30839898923264,1.52771686646453,1.82014070277373),
 .UNSPECIFIED.);
#386=B_SPLINE_CURVE_WITH_KNOTS('',3,(#30756,#30757,#30758,#30759),
 .UNSPECIFIED.,.F.,.F.,(4,4),(1.25128936731019,1.30839898923273),
 .UNSPECIFIED.);
#387=B_SPLINE_CURVE_WITH_KNOTS('',3,(#30763,#30764,#30765,#30766),
 .UNSPECIFIED.,.F.,.F.,(4,4),(0.511841573844537,0.568951195767077),
 .UNSPECIFIED.);
#388=B_SPLINE_CURVE_WITH_KNOTS('',3,(#30780,#30781,#30782,#30783,#30784,
#30785,#30786,#30787,#30788,#30789,#30790,#30791,#30792,#30793,#30794,#30795,
#30796,#30797,#30798,#30799,#30800,#30801,#30802,#30803,#30804,#30805,#30806,
#30807,#30808,#30809,#30810,#30811,#30812,#30813,#30814,#30815,#30816,#30817,
#30818,#30819,#30820,#30821,#30822,#30823,#30824,#30825,#30826,#30827,#30828,
#30829,#30830,#30831,#30832,#30833,#30834,#30835,#30836,#30837,#30838,#30839,
#30840,#30841,#30842,#30843,#30844,#30845,#30846,#30847,#30848,#30849),
 .UNSPECIFIED.,.F.,.F.,(4,3,3,3,3,3,3,3,3,3,3,3,3,3,3,3,3,3,3,3,3,3,3,4),
(0.,0.0359049130301229,0.073176546683956,0.112193891804418,0.153584180872903,
0.198557499184731,0.251370834104054,0.322351740640927,0.369695706937292,
0.412227002231532,0.451956927695583,0.490325801015499,0.529954282797085,
0.570193681578136,0.613255160380649,0.661188818329747,0.72826172337588,
0.783705946924147,0.829760857074988,0.872320642806241,0.910999990516432,
0.948303454885518,0.984018194834891,1.),.UNSPECIFIED.);
#389=B_SPLINE_CURVE_WITH_KNOTS('',3,(#30894,#30895,#30896,#30897,#30898,
#30899,#30900,#30901,#30902,#30903,#30904,#30905,#30906,#30907,#30908,#30909,
#30910,#30911,#30912,#30913,#30914,#30915,#30916,#30917,#30918,#30919,#30920,
#30921,#30922,#30923,#30924,#30925,#30926,#30927,#30928,#30929,#30930,#30931,
#30932,#30933,#30934,#30935,#30936,#30937,#30938,#30939,#30940,#30941,#30942,
#30943,#30944,#30945,#30946,#30947,#30948,#30949,#30950,#30951,#30952,#30953,
#30954,#30955,#30956,#30957,#30958,#30959,#30960,#30961,#30962,#30963,#30964,
#30965,#30966,#30967,#30968,#30969,#30970,#30971,#30972,#30973,#30974,#30975,
#30976,#30977,#30978,#30979,#30980,#30981,#30982,#30983,#30984,#30985,#30986,
#30987),.UNSPECIFIED.,.F.,.F.,(4,3,3,3,3,3,3,3,3,3,3,3,3,3,3,3,3,3,3,3,
3,3,3,3,3,3,3,3,3,3,3,4),(0.,0.0258707373554823,0.0523995840965019,0.0797001062399438,
0.108495122304716,0.13857954762218,0.170391094064582,0.204740917510112,
0.243564929276073,0.301738532460215,0.342786817991936,0.377562326039311,
0.409462752131609,0.4395237743171,0.468248826864701,0.497342037419088,0.525270551060381,
0.554941141619107,0.585586423719045,0.618112002054742,0.653483629073077,
0.694829907664093,0.747358418123701,0.784774066856292,0.818382574947157,
0.849773403889227,0.879622022458522,0.909716516843892,0.937043933517235,
0.963754511581492,0.989696243099283,1.),.UNSPECIFIED.);
#390=B_SPLINE_CURVE_WITH_KNOTS('',3,(#30989,#30990,#30991,#30992),
 .UNSPECIFIED.,.F.,.F.,(4,4),(-1.,0.),.UNSPECIFIED.);
#391=B_SPLINE_CURVE_WITH_KNOTS('',3,(#30994,#30995,#30996,#30997,#30998,
#30999,#31000,#31001,#31002,#31003,#31004,#31005,#31006,#31007,#31008,#31009,
#31010,#31011,#31012,#31013,#31014,#31015,#31016,#31017,#31018,#31019,#31020,
#31021,#31022,#31023,#31024,#31025,#31026,#31027,#31028,#31029,#31030,#31031,
#31032,#31033,#31034,#31035,#31036,#31037,#31038,#31039,#31040,#31041,#31042,
#31043,#31044,#31045,#31046,#31047,#31048,#31049,#31050,#31051,#31052,#31053,
#31054,#31055,#31056,#31057,#31058,#31059,#31060,#31061,#31062,#31063),
 .UNSPECIFIED.,.F.,.F.,(4,3,3,3,3,3,3,3,3,3,3,3,3,3,3,3,3,3,3,3,3,3,3,4),
(0.,0.0359057505369141,0.0731783002803435,0.112196677628097,0.153588190534333,
0.19856311454628,0.251379999966526,0.322351119348276,0.369695904752862,
0.412227932090299,0.451958540119749,0.490327995227232,0.529955242586758,
0.570194130838204,0.613255080635413,0.66118816290105,0.728261099602057,
0.783703930049219,0.829758027567063,0.872318520675297,0.910997186415849,
0.948300017650692,0.984014136985868,1.),.UNSPECIFIED.);
#392=B_SPLINE_CURVE_WITH_KNOTS('',3,(#31099,#31100,#31101,#31102,#31103,
#31104,#31105,#31106,#31107,#31108,#31109,#31110,#31111,#31112,#31113,#31114,
#31115,#31116,#31117,#31118,#31119,#31120,#31121,#31122,#31123,#31124,#31125,
#31126,#31127,#31128,#31129,#31130,#31131,#31132,#31133,#31134,#31135,#31136,
#31137,#31138,#31139,#31140,#31141,#31142,#31143,#31144,#31145,#31146,#31147,
#31148,#31149,#31150,#31151,#31152,#31153,#31154,#31155,#31156,#31157,#31158,
#31159,#31160,#31161,#31162,#31163,#31164,#31165,#31166,#31167,#31168),
 .UNSPECIFIED.,.F.,.F.,(4,3,3,3,3,3,3,3,3,3,3,3,3,3,3,3,3,3,3,3,3,3,3,4),
(0.,0.0359049130299729,0.0731765466835763,0.112193891804017,0.153584180872098,
0.198557499183881,0.251370834102748,0.322351740640327,0.369695706936552,
0.41222700223062,0.451956927694618,0.490325801013735,0.529954282795424,
0.570193681576247,0.613255160378796,0.661188818327897,0.728261723370456,
0.783705946920119,0.829760857071578,0.872320642803683,0.910999990513864,
0.948303454883392,0.984018194832596,1.),.UNSPECIFIED.);
#393=B_SPLINE_CURVE_WITH_KNOTS('',3,(#31170,#31171,#31172,#31173),
 .UNSPECIFIED.,.F.,.F.,(4,4),(0.,1.),.UNSPECIFIED.);
#394=B_SPLINE_CURVE_WITH_KNOTS('',3,(#31175,#31176,#31177,#31178,#31179,
#31180,#31181,#31182,#31183,#31184,#31185,#31186,#31187,#31188,#31189,#31190,
#31191,#31192,#31193,#31194,#31195,#31196,#31197,#31198,#31199,#31200,#31201,
#31202,#31203,#31204,#31205,#31206,#31207,#31208,#31209,#31210,#31211,#31212,
#31213,#31214,#31215,#31216,#31217,#31218,#31219,#31220,#31221,#31222,#31223,
#31224,#31225,#31226,#31227,#31228,#31229,#31230,#31231,#31232,#31233,#31234,
#31235,#31236,#31237,#31238,#31239,#31240,#31241,#31242,#31243,#31244,#31245,
#31246,#31247,#31248,#31249,#31250,#31251,#31252,#31253,#31254,#31255,#31256,
#31257,#31258,#31259,#31260,#31261,#31262,#31263,#31264,#31265,#31266,#31267,
#31268),.UNSPECIFIED.,.F.,.F.,(4,3,3,3,3,3,3,3,3,3,3,3,3,3,3,3,3,3,3,3,
3,3,3,3,3,3,3,3,3,3,3,4),(0.,0.0258806756174258,0.052420092429605,0.0797320054697036,
0.108539986218788,0.138639210368191,0.170468543243868,0.204841963556246,
0.243705622058159,0.301747781272309,0.342801248093589,0.377583660478043,
0.409491201673175,0.439559325359787,0.468291402624354,0.497246494854993,
0.525185051724753,0.554860985991956,0.585493448014801,0.618003831060507,
0.653355385806342,0.694654047173711,0.747235197965173,0.78464773063489,
0.818250753894271,0.849635401976391,0.879477590190491,0.909608192642869,
0.936927406576889,0.963630039350146,0.989563298296144,1.),.UNSPECIFIED.);
#395=B_SPLINE_CURVE_WITH_KNOTS('',3,(#31291,#31292,#31293,#31294,#31295),
 .UNSPECIFIED.,.F.,.F.,(4,1,4),(0.000100085581199305,0.2925237931603,0.511841573844626),
 .UNSPECIFIED.);
#396=B_SPLINE_CURVE_WITH_KNOTS('',3,(#31297,#31298,#31299,#31300,#31301),
 .UNSPECIFIED.,.F.,.F.,(4,1,4),(-0.511841573844626,-0.2925237931603,-0.000100085581199305),
 .UNSPECIFIED.);
#397=B_SPLINE_CURVE_WITH_KNOTS('',3,(#31324,#31325,#31326,#31327),
 .UNSPECIFIED.,.F.,.F.,(4,4),(0.511841573844536,0.568951195767079),
 .UNSPECIFIED.);
#398=B_SPLINE_CURVE_WITH_KNOTS('',3,(#31348,#31349,#31350,#31351,#31352),
 .UNSPECIFIED.,.F.,.F.,(4,1,4),(-1.80301165508774,-1.58369377785584,-1.29126994154665),
 .UNSPECIFIED.);
#399=B_SPLINE_CURVE_WITH_KNOTS('',3,(#31355,#31356,#31357,#31358,#31359),
 .UNSPECIFIED.,.F.,.F.,(4,1,4),(1.29126994154665,1.58369377785584,1.80301165508774),
 .UNSPECIFIED.);
#400=B_SPLINE_CURVE_WITH_KNOTS('',3,(#31376,#31377,#31378,#31379),
 .UNSPECIFIED.,.F.,.F.,(4,4),(1.2341603196242,1.29126994154674),
 .UNSPECIFIED.);
#401=B_SPLINE_CURVE_WITH_KNOTS('',3,(#31428,#31429,#31430,#31431,#31432,
#31433,#31434,#31435,#31436,#31437,#31438,#31439,#31440,#31441,#31442,#31443,
#31444,#31445,#31446,#31447,#31448,#31449,#31450,#31451,#31452,#31453,#31454,
#31455,#31456,#31457,#31458,#31459,#31460,#31461,#31462,#31463,#31464,#31465,
#31466,#31467,#31468,#31469,#31470,#31471,#31472,#31473,#31474,#31475,#31476,
#31477,#31478,#31479,#31480,#31481,#31482,#31483,#31484,#31485,#31486,#31487,
#31488,#31489,#31490,#31491,#31492,#31493,#31494,#31495,#31496,#31497,#31498,
#31499,#31500,#31501,#31502,#31503,#31504,#31505,#31506,#31507,#31508,#31509,
#31510,#31511,#31512,#31513,#31514,#31515,#31516,#31517,#31518,#31519,#31520,
#31521),.UNSPECIFIED.,.F.,.F.,(4,3,3,3,3,3,3,3,3,3,3,3,3,3,3,3,3,3,3,3,
3,3,3,3,3,3,3,3,3,3,3,4),(0.,0.0258707373851967,0.0523995841581851,0.0797001063345152,
0.108495122436992,0.138579547796862,0.17039109428924,0.204740917798925,
0.243564929673233,0.301738533531212,0.342786818919031,0.377562326926076,
0.409462753001591,0.439523775181584,0.468248827730322,0.497342036568899,
0.525270550411958,0.554941141011211,0.585586423119647,0.618112001453771,
0.653483628441857,0.694829906775598,0.747358417163864,0.784774066049438,
0.818382574241438,0.849773403260588,0.879622021894085,0.909716516420564,
0.937043933139874,0.963754511247475,0.98969624280447,1.),.UNSPECIFIED.);
#402=B_SPLINE_CURVE_WITH_KNOTS('',3,(#31522,#31523,#31524,#31525),
 .UNSPECIFIED.,.F.,.F.,(4,4),(-1.,0.),.UNSPECIFIED.);
#403=B_SPLINE_CURVE_WITH_KNOTS('',3,(#31560,#31561,#31562,#31563),
 .UNSPECIFIED.,.F.,.F.,(4,4),(0.,1.),.UNSPECIFIED.);
#404=B_SPLINE_CURVE_WITH_KNOTS('',3,(#31564,#31565,#31566,#31567,#31568,
#31569,#31570,#31571,#31572,#31573,#31574,#31575,#31576,#31577,#31578,#31579,
#31580,#31581,#31582,#31583,#31584,#31585,#31586,#31587,#31588,#31589,#31590,
#31591,#31592,#31593,#31594,#31595,#31596,#31597,#31598,#31599,#31600,#31601,
#31602,#31603,#31604,#31605,#31606,#31607,#31608,#31609,#31610,#31611,#31612,
#31613,#31614,#31615,#31616,#31617,#31618,#31619,#31620,#31621,#31622,#31623,
#31624,#31625,#31626,#31627,#31628,#31629,#31630,#31631,#31632,#31633,#31634,
#31635,#31636,#31637,#31638,#31639,#31640,#31641,#31642,#31643,#31644,#31645,
#31646,#31647,#31648,#31649,#31650,#31651,#31652,#31653,#31654,#31655,#31656,
#31657),.UNSPECIFIED.,.F.,.F.,(4,3,3,3,3,3,3,3,3,3,3,3,3,3,3,3,3,3,3,3,
3,3,3,3,3,3,3,3,3,3,3,4),(0.,0.0258806756174331,0.0524200924297352,0.0797320054696585,
0.108539986218731,0.13863921036807,0.170468543243706,0.204841963556146,
0.243705622058077,0.301747781273792,0.342801248094138,0.377583660478468,
0.409491201673628,0.439559325360195,0.468291402624606,0.497246494854655,
0.52518505172447,0.554860985991691,0.585493448014516,0.61800383106021,0.653355385806122,
0.694654047173536,0.747235197964895,0.784647730634614,0.818250753893958,
0.849635401976054,0.879477590190265,0.909608192642699,0.936927406576695,
0.963630039349939,0.989563298295856,1.),.UNSPECIFIED.);
#405=B_SPLINE_CURVE_WITH_KNOTS('',3,(#31679,#31680,#31681,#31682,#31683),
 .UNSPECIFIED.,.F.,.F.,(4,1,4),(-0.511841573844627,-0.292523793160301,-0.000100085581199306),
 .UNSPECIFIED.);
#406=B_SPLINE_CURVE_WITH_KNOTS('',3,(#31723,#31724,#31725,#31726,#31727),
 .UNSPECIFIED.,.F.,.F.,(4,1,4),(-1.82014070277373,-1.52771686646453,-1.30839898923264),
 .UNSPECIFIED.);
#407=B_SPLINE_SURFACE_WITH_KNOTS('',3,3,((#18612,#18613,#18614,#18615,#18616),
(#18617,#18618,#18619,#18620,#18621),(#18622,#18623,#18624,#18625,#18626),
(#18627,#18628,#18629,#18630,#18631)),.UNSPECIFIED.,.F.,.F.,.F.,(4,4),(4,
1,4),(0.,1.),(0.,0.571428571428571,1.),.UNSPECIFIED.);
#408=B_SPLINE_SURFACE_WITH_KNOTS('',3,3,((#18775,#18776,#18777,#18778,#18779,
#18780,#18781,#18782,#18783),(#18784,#18785,#18786,#18787,#18788,#18789,
#18790,#18791,#18792),(#18793,#18794,#18795,#18796,#18797,#18798,#18799,
#18800,#18801),(#18802,#18803,#18804,#18805,#18806,#18807,#18808,#18809,
#18810)),.UNSPECIFIED.,.F.,.F.,.F.,(4,4),(4,1,1,1,1,1,4),(0.,1.),(0.,0.214285714285714,
0.357142857142857,0.571428571428571,0.785714285714286,0.857142857142857,
1.),.UNSPECIFIED.);
#409=B_SPLINE_SURFACE_WITH_KNOTS('',3,3,((#18954,#18955,#18956,#18957,#18958,
#18959),(#18960,#18961,#18962,#18963,#18964,#18965),(#18966,#18967,#18968,
#18969,#18970,#18971),(#18972,#18973,#18974,#18975,#18976,#18977)),
 .UNSPECIFIED.,.F.,.F.,.F.,(4,4),(4,2,4),(0.,1.),(9.99629094513137E-5,0.155241085196768,
0.273153287835105),.UNSPECIFIED.);
#410=B_SPLINE_SURFACE_WITH_KNOTS('',3,3,((#19002,#19003,#19004,#19005),
(#19006,#19007,#19008,#19009),(#19010,#19011,#19012,#19013),(#19014,#19015,
#19016,#19017)),.UNSPECIFIED.,.F.,.F.,.F.,(4,4),(4,4),(0.,1.),(0.273153287835093,
0.310482170393534),.UNSPECIFIED.);
#411=B_SPLINE_SURFACE_WITH_KNOTS('',3,3,((#19026,#19027,#19028,#19029,#19030,
#19031),(#19032,#19033,#19034,#19035,#19036,#19037),(#19038,#19039,#19040,
#19041,#19042,#19043),(#19044,#19045,#19046,#19047,#19048,#19049)),
 .UNSPECIFIED.,.F.,.F.,.F.,(4,4),(4,2,4),(0.,1.),(0.681237813527798,0.799150016166132,
0.954291288267864),.UNSPECIFIED.);
#412=B_SPLINE_SURFACE_WITH_KNOTS('',3,3,((#19065,#19066,#19067,#19068),
(#19069,#19070,#19071,#19072),(#19073,#19074,#19075,#19076),(#19077,#19078,
#19079,#19080)),.UNSPECIFIED.,.F.,.F.,.F.,(4,4),(4,4),(0.,1.),(0.643908930969367,
0.681237813527811),.UNSPECIFIED.);
#413=B_SPLINE_SURFACE_WITH_KNOTS('',3,3,((#19329,#19330,#19331,#19332,#19333),
(#19334,#19335,#19336,#19337,#19338),(#19339,#19340,#19341,#19342,#19343),
(#19344,#19345,#19346,#19347,#19348)),.UNSPECIFIED.,.F.,.F.,.F.,(4,4),(4,
1,4),(0.,1.),(0.,0.571428571428571,1.),.UNSPECIFIED.);
#414=B_SPLINE_SURFACE_WITH_KNOTS('',3,3,((#19492,#19493,#19494,#19495,#19496,
#19497,#19498,#19499,#19500),(#19501,#19502,#19503,#19504,#19505,#19506,
#19507,#19508,#19509),(#19510,#19511,#19512,#19513,#19514,#19515,#19516,
#19517,#19518),(#19519,#19520,#19521,#19522,#19523,#19524,#19525,#19526,
#19527)),.UNSPECIFIED.,.F.,.F.,.F.,(4,4),(4,1,1,1,1,1,4),(0.,1.),(0.,0.214285714285714,
0.357142857142857,0.571428571428571,0.785714285714286,0.857142857142857,
1.),.UNSPECIFIED.);
#415=B_SPLINE_SURFACE_WITH_KNOTS('',3,3,((#19585,#19586,#19587,#19588,#19589,
#19590),(#19591,#19592,#19593,#19594,#19595,#19596),(#19597,#19598,#19599,
#19600,#19601,#19602),(#19603,#19604,#19605,#19606,#19607,#19608)),
 .UNSPECIFIED.,.F.,.F.,.F.,(4,4),(4,2,4),(0.,1.),(9.99629094513097E-5,0.155241085196768,
0.273153287835103),.UNSPECIFIED.);
#416=B_SPLINE_SURFACE_WITH_KNOTS('',3,3,((#19626,#19627,#19628,#19629),
(#19630,#19631,#19632,#19633),(#19634,#19635,#19636,#19637),(#19638,#19639,
#19640,#19641)),.UNSPECIFIED.,.F.,.F.,.F.,(4,4),(4,4),(0.,1.),(0.273153287835089,
0.310482170393536),.UNSPECIFIED.);
#417=B_SPLINE_SURFACE_WITH_KNOTS('',3,3,((#19650,#19651,#19652,#19653,#19654,
#19655),(#19656,#19657,#19658,#19659,#19660,#19661),(#19662,#19663,#19664,
#19665,#19666,#19667),(#19668,#19669,#19670,#19671,#19672,#19673)),
 .UNSPECIFIED.,.F.,.F.,.F.,(4,4),(4,2,4),(0.,1.),(0.675695431302217,0.778344160365421,
0.945184496035906),.UNSPECIFIED.);
#418=B_SPLINE_SURFACE_WITH_KNOTS('',3,3,((#19689,#19690,#19691,#19692),
(#19693,#19694,#19695,#19696),(#19697,#19698,#19699,#19700),(#19701,#19702,
#19703,#19704)),.UNSPECIFIED.,.F.,.F.,.F.,(4,4),(4,4),(0.,1.),(0.639351607098029,
0.675695431302254),.UNSPECIFIED.);
#419=B_SPLINE_SURFACE_WITH_KNOTS('',3,3,((#19723,#19724,#19725,#19726,#19727),
(#19728,#19729,#19730,#19731,#19732),(#19733,#19734,#19735,#19736,#19737),
(#19738,#19739,#19740,#19741,#19742)),.UNSPECIFIED.,.F.,.F.,.F.,(4,4),(4,
1,4),(0.,1.),(0.,0.571428571428571,1.),.UNSPECIFIED.);
#420=B_SPLINE_SURFACE_WITH_KNOTS('',3,3,((#19883,#19884,#19885,#19886,#19887,
#19888,#19889,#19890,#19891),(#19892,#19893,#19894,#19895,#19896,#19897,
#19898,#19899,#19900),(#19901,#19902,#19903,#19904,#19905,#19906,#19907,
#19908,#19909),(#19910,#19911,#19912,#19913,#19914,#19915,#19916,#19917,
#19918)),.UNSPECIFIED.,.F.,.F.,.F.,(4,4),(4,1,1,1,1,1,4),(0.,1.),(0.,0.214285714285714,
0.357142857142857,0.571428571428571,0.785714285714286,0.857142857142857,
1.),.UNSPECIFIED.);
#421=B_SPLINE_SURFACE_WITH_KNOTS('',3,3,((#20062,#20063,#20064,#20065,#20066,
#20067),(#20068,#20069,#20070,#20071,#20072,#20073),(#20074,#20075,#20076,
#20077,#20078,#20079),(#20080,#20081,#20082,#20083,#20084,#20085)),
 .UNSPECIFIED.,.F.,.F.,.F.,(4,4),(4,2,4),(0.,1.),(9.99629094513175E-5,0.155241085196768,
0.273153287835103),.UNSPECIFIED.);
#422=B_SPLINE_SURFACE_WITH_KNOTS('',3,3,((#20110,#20111,#20112,#20113),
(#20114,#20115,#20116,#20117),(#20118,#20119,#20120,#20121),(#20122,#20123,
#20124,#20125)),.UNSPECIFIED.,.F.,.F.,.F.,(4,4),(4,4),(0.,1.),(0.273153287835089,
0.310482170393535),.UNSPECIFIED.);
#423=B_SPLINE_SURFACE_WITH_KNOTS('',3,3,((#20134,#20135,#20136,#20137,#20138,
#20139),(#20140,#20141,#20142,#20143,#20144,#20145),(#20146,#20147,#20148,
#20149,#20150,#20151),(#20152,#20153,#20154,#20155,#20156,#20157)),
 .UNSPECIFIED.,.F.,.F.,.F.,(4,4),(4,2,4),(0.,1.),(0.67569543130222,0.778344160365423,
0.945184496035905),.UNSPECIFIED.);
#424=B_SPLINE_SURFACE_WITH_KNOTS('',3,3,((#20173,#20174,#20175,#20176),
(#20177,#20178,#20179,#20180),(#20181,#20182,#20183,#20184),(#20185,#20186,
#20187,#20188)),.UNSPECIFIED.,.F.,.F.,.F.,(4,4),(4,4),(0.,1.),(0.639351607098027,
0.675695431302257),.UNSPECIFIED.);
#425=B_SPLINE_SURFACE_WITH_KNOTS('',3,3,((#20291,#20292,#20293,#20294,#20295),
(#20296,#20297,#20298,#20299,#20300),(#20301,#20302,#20303,#20304,#20305),
(#20306,#20307,#20308,#20309,#20310)),.UNSPECIFIED.,.F.,.F.,.F.,(4,4),(4,
1,4),(0.,1.),(0.,0.571428571428571,1.),.UNSPECIFIED.);
#426=B_SPLINE_SURFACE_WITH_KNOTS('',3,3,((#20400,#20401,#20402,#20403,#20404,
#20405,#20406,#20407,#20408),(#20409,#20410,#20411,#20412,#20413,#20414,
#20415,#20416,#20417),(#20418,#20419,#20420,#20421,#20422,#20423,#20424,
#20425,#20426),(#20427,#20428,#20429,#20430,#20431,#20432,#20433,#20434,
#20435)),.UNSPECIFIED.,.F.,.F.,.F.,(4,4),(4,1,1,1,1,1,4),(0.,1.),(0.,0.214285714285714,
0.357142857142857,0.571428571428571,0.785714285714286,0.857142857142857,
1.),.UNSPECIFIED.);
#427=B_SPLINE_SURFACE_WITH_KNOTS('',3,3,((#20440,#20441,#20442,#20443,#20444,
#20445),(#20446,#20447,#20448,#20449,#20450,#20451),(#20452,#20453,#20454,
#20455,#20456,#20457),(#20458,#20459,#20460,#20461,#20462,#20463)),
 .UNSPECIFIED.,.F.,.F.,.F.,(4,4),(4,2,4),(0.,1.),(9.97881403247492E-5,0.166940126137213,
0.269588855200419),.UNSPECIFIED.);
#428=B_SPLINE_SURFACE_WITH_KNOTS('',3,3,((#20471,#20472,#20473,#20474),
(#20475,#20476,#20477,#20478),(#20479,#20480,#20481,#20482),(#20483,#20484,
#20485,#20486)),.UNSPECIFIED.,.F.,.F.,.F.,(4,4),(4,4),(0.,1.),(0.269588855200382,
0.305932679404608),.UNSPECIFIED.);
#429=B_SPLINE_SURFACE_WITH_KNOTS('',3,3,((#20491,#20492,#20493,#20494,#20495,
#20496),(#20497,#20498,#20499,#20500,#20501,#20502),(#20503,#20504,#20505,
#20506,#20507,#20508),(#20509,#20510,#20511,#20512,#20513,#20514)),
 .UNSPECIFIED.,.F.,.F.,.F.,(4,4),(4,2,4),(0.,1.),(0.681229980645395,0.79914218328373,
0.954283455385462),.UNSPECIFIED.);
#430=B_SPLINE_SURFACE_WITH_KNOTS('',3,3,((#20523,#20524,#20525,#20526),
(#20527,#20528,#20529,#20530),(#20531,#20532,#20533,#20534),(#20535,#20536,
#20537,#20538)),.UNSPECIFIED.,.F.,.F.,.F.,(4,4),(4,4),(0.,1.),(0.643901098086962,
0.681229980645409),.UNSPECIFIED.);
#431=B_SPLINE_SURFACE_WITH_KNOTS('',3,3,((#20631,#20632,#20633,#20634,#20635,
#20636),(#20637,#20638,#20639,#20640,#20641,#20642),(#20643,#20644,#20645,
#20646,#20647,#20648),(#20649,#20650,#20651,#20652,#20653,#20654)),
 .UNSPECIFIED.,.F.,.F.,.F.,(4,4),(4,1,1,4),(0.,1.),(0.,0.571428571428571,
0.857142857142857,1.),.UNSPECIFIED.);
#432=B_SPLINE_SURFACE_WITH_KNOTS('',3,3,((#20756,#20757,#20758,#20759,#20760,
#20761),(#20762,#20763,#20764,#20765,#20766,#20767),(#20768,#20769,#20770,
#20771,#20772,#20773),(#20774,#20775,#20776,#20777,#20778,#20779)),
 .UNSPECIFIED.,.F.,.F.,.F.,(4,4),(4,1,1,4),(0.,1.),(0.,0.571428571428571,
0.857142857142857,1.),.UNSPECIFIED.);
#433=B_SPLINE_SURFACE_WITH_KNOTS('',3,3,((#20881,#20882,#20883,#20884,#20885,
#20886,#20887),(#20888,#20889,#20890,#20891,#20892,#20893,#20894),(#20895,
#20896,#20897,#20898,#20899,#20900,#20901),(#20902,#20903,#20904,#20905,
#20906,#20907,#20908)),.UNSPECIFIED.,.F.,.F.,.F.,(4,4),(4,1,1,1,4),(0.,
1.),(-1.70953476876621,-1.22109626340444,-0.732657758042664,-0.366328879021332,
5.55111512312578E-17),.UNSPECIFIED.);
#434=B_SPLINE_SURFACE_WITH_KNOTS('',3,3,((#20932,#20933,#20934,#20935,#20936,
#20937),(#20938,#20939,#20940,#20941,#20942,#20943),(#20944,#20945,#20946,
#20947,#20948,#20949),(#20950,#20951,#20952,#20953,#20954,#20955)),
 .UNSPECIFIED.,.F.,.F.,.F.,(4,4),(4,1,1,4),(0.,1.),(-1.70953476876627,-0.976877010723583,
-0.488438505361791,0.),.UNSPECIFIED.);
#435=B_SPLINE_SURFACE_WITH_KNOTS('',3,3,((#21098,#21099,#21100,#21101,#21102,
#21103),(#21104,#21105,#21106,#21107,#21108,#21109),(#21110,#21111,#21112,
#21113,#21114,#21115),(#21116,#21117,#21118,#21119,#21120,#21121)),
 .UNSPECIFIED.,.F.,.F.,.F.,(4,4),(4,1,1,4),(0.,1.),(0.,0.571428571428571,
0.857142857142857,1.),.UNSPECIFIED.);
#436=B_SPLINE_SURFACE_WITH_KNOTS('',3,3,((#21175,#21176,#21177,#21178,#21179,
#21180),(#21181,#21182,#21183,#21184,#21185,#21186),(#21187,#21188,#21189,
#21190,#21191,#21192),(#21193,#21194,#21195,#21196,#21197,#21198)),
 .UNSPECIFIED.,.F.,.F.,.F.,(4,4),(4,1,1,4),(0.,1.),(0.,0.571428571428571,
0.857142857142857,1.),.UNSPECIFIED.);
#437=B_SPLINE_SURFACE_WITH_KNOTS('',3,3,((#21250,#21251,#21252,#21253,#21254,
#21255),(#21256,#21257,#21258,#21259,#21260,#21261),(#21262,#21263,#21264,
#21265,#21266,#21267),(#21268,#21269,#21270,#21271,#21272,#21273)),
 .UNSPECIFIED.,.F.,.F.,.F.,(4,4),(4,1,1,4),(0.,1.),(-1.70953476876622,-0.976877010723545,
-0.488438505361761,2.2204460492503E-14),.UNSPECIFIED.);
#438=B_SPLINE_SURFACE_WITH_KNOTS('',3,3,((#21286,#21287,#21288,#21289,#21290,
#21291),(#21292,#21293,#21294,#21295,#21296,#21297),(#21298,#21299,#21300,
#21301,#21302,#21303),(#21304,#21305,#21306,#21307,#21308,#21309)),
 .UNSPECIFIED.,.F.,.F.,.F.,(4,4),(4,1,1,4),(0.,1.),(-1.70953476876625,-0.976877010723563,
-0.48843850536177,2.22044604925036E-14),.UNSPECIFIED.);
#439=B_SPLINE_SURFACE_WITH_KNOTS('',3,3,((#21432,#21433,#21434,#21435,#21436,
#21437),(#21438,#21439,#21440,#21441,#21442,#21443),(#21444,#21445,#21446,
#21447,#21448,#21449),(#21450,#21451,#21452,#21453,#21454,#21455)),
 .UNSPECIFIED.,.F.,.F.,.F.,(4,4),(4,1,1,4),(0.,1.),(0.,0.571428571428571,
0.857142857142857,1.),.UNSPECIFIED.);
#440=B_SPLINE_SURFACE_WITH_KNOTS('',3,3,((#21507,#21508,#21509,#21510,#21511,
#21512),(#21513,#21514,#21515,#21516,#21517,#21518),(#21519,#21520,#21521,
#21522,#21523,#21524),(#21525,#21526,#21527,#21528,#21529,#21530)),
 .UNSPECIFIED.,.F.,.F.,.F.,(4,4),(4,1,1,4),(0.,1.),(0.,0.571428571428571,
0.857142857142857,1.),.UNSPECIFIED.);
#441=B_SPLINE_SURFACE_WITH_KNOTS('',3,3,((#21584,#21585,#21586,#21587,#21588,
#21589),(#21590,#21591,#21592,#21593,#21594,#21595),(#21596,#21597,#21598,
#21599,#21600,#21601),(#21602,#21603,#21604,#21605,#21606,#21607)),
 .UNSPECIFIED.,.F.,.F.,.F.,(4,4),(4,1,1,4),(0.,1.),(-1.70953476876624,-0.976877010723568,
-0.488438505361784,0.),.UNSPECIFIED.);
#442=B_SPLINE_SURFACE_WITH_KNOTS('',3,3,((#21620,#21621,#21622,#21623,#21624,
#21625),(#21626,#21627,#21628,#21629,#21630,#21631),(#21632,#21633,#21634,
#21635,#21636,#21637),(#21638,#21639,#21640,#21641,#21642,#21643)),
 .UNSPECIFIED.,.F.,.F.,.F.,(4,4),(4,1,1,4),(0.,1.),(-1.70953476876623,-0.976877010723558,
-0.488438505361779,0.),.UNSPECIFIED.);
#443=B_SPLINE_SURFACE_WITH_KNOTS('',3,3,((#21650,#21651,#21652,#21653,#21654,
#21655),(#21656,#21657,#21658,#21659,#21660,#21661),(#21662,#21663,#21664,
#21665,#21666,#21667),(#21668,#21669,#21670,#21671,#21672,#21673)),
 .UNSPECIFIED.,.F.,.F.,.F.,(4,4),(4,1,1,4),(0.,1.),(0.,0.571428571428571,
0.857142857142857,1.),.UNSPECIFIED.);
#444=B_SPLINE_SURFACE_WITH_KNOTS('',3,3,((#21772,#21773,#21774,#21775,#21776,
#21777),(#21778,#21779,#21780,#21781,#21782,#21783),(#21784,#21785,#21786,
#21787,#21788,#21789),(#21790,#21791,#21792,#21793,#21794,#21795)),
 .UNSPECIFIED.,.F.,.F.,.F.,(4,4),(4,1,1,4),(0.,1.),(0.,0.571428571428571,
0.857142857142857,1.),.UNSPECIFIED.);
#445=B_SPLINE_SURFACE_WITH_KNOTS('',3,3,((#21897,#21898,#21899,#21900,#21901,
#21902),(#21903,#21904,#21905,#21906,#21907,#21908),(#21909,#21910,#21911,
#21912,#21913,#21914),(#21915,#21916,#21917,#21918,#21919,#21920)),
 .UNSPECIFIED.,.F.,.F.,.F.,(4,4),(4,1,1,4),(0.,1.),(-1.7095347687662,-0.97687701072354,
-0.488438505361764,1.11854969730985E-14),.UNSPECIFIED.);
#446=B_SPLINE_SURFACE_WITH_KNOTS('',3,3,((#21942,#21943,#21944,#21945,#21946,
#21947),(#21948,#21949,#21950,#21951,#21952,#21953),(#21954,#21955,#21956,
#21957,#21958,#21959),(#21960,#21961,#21962,#21963,#21964,#21965)),
 .UNSPECIFIED.,.F.,.F.,.F.,(4,4),(4,1,1,4),(0.,1.),(-3.1415926535898,-2.65315414822802,
-2.16471564286623,-1.43205788482356),.UNSPECIFIED.);
#447=B_SPLINE_SURFACE_WITH_KNOTS('',3,3,((#22642,#22643,#22644,#22645,#22646),
(#22647,#22648,#22649,#22650,#22651),(#22652,#22653,#22654,#22655,#22656),
(#22657,#22658,#22659,#22660,#22661)),.UNSPECIFIED.,.F.,.F.,.F.,(4,4),(4,
1,4),(0.,1.),(0.,0.571428571428571,1.),.UNSPECIFIED.);
#448=B_SPLINE_SURFACE_WITH_KNOTS('',3,3,((#22805,#22806,#22807,#22808,#22809,
#22810,#22811,#22812,#22813),(#22814,#22815,#22816,#22817,#22818,#22819,
#22820,#22821,#22822),(#22823,#22824,#22825,#22826,#22827,#22828,#22829,
#22830,#22831),(#22832,#22833,#22834,#22835,#22836,#22837,#22838,#22839,
#22840)),.UNSPECIFIED.,.F.,.F.,.F.,(4,4),(4,1,1,1,1,1,4),(0.,1.),(0.,0.214285714285714,
0.357142857142857,0.571428571428571,0.785714285714286,0.857142857142857,
1.),.UNSPECIFIED.);
#449=B_SPLINE_SURFACE_WITH_KNOTS('',3,3,((#22984,#22985,#22986,#22987),
(#22988,#22989,#22990,#22991),(#22992,#22993,#22994,#22995),(#22996,#22997,
#22998,#22999)),.UNSPECIFIED.,.F.,.F.,.F.,(4,4),(4,4),(0.,1.),(9.99629094513139E-5,
0.273153287835102),.UNSPECIFIED.);
#450=B_SPLINE_SURFACE_WITH_KNOTS('',3,3,((#23020,#23021,#23022,#23023),
(#23024,#23025,#23026,#23027),(#23028,#23029,#23030,#23031),(#23032,#23033,
#23034,#23035)),.UNSPECIFIED.,.F.,.F.,.F.,(4,4),(4,4),(0.,1.),(0.273153287835088,
0.310482170393536),.UNSPECIFIED.);
#451=B_SPLINE_SURFACE_WITH_KNOTS('',3,3,((#23044,#23045,#23046,#23047,#23048,
#23049),(#23050,#23051,#23052,#23053,#23054,#23055),(#23056,#23057,#23058,
#23059,#23060,#23061),(#23062,#23063,#23064,#23065,#23066,#23067)),
 .UNSPECIFIED.,.F.,.F.,.F.,(4,4),(4,2,4),(0.,1.),(0.681237813527804,0.799150016166134,
0.954291288267866),.UNSPECIFIED.);
#452=B_SPLINE_SURFACE_WITH_KNOTS('',3,3,((#23083,#23084,#23085,#23086),
(#23087,#23088,#23089,#23090),(#23091,#23092,#23093,#23094),(#23095,#23096,
#23097,#23098)),.UNSPECIFIED.,.F.,.F.,.F.,(4,4),(4,4),(0.,1.),(0.643908930969367,
0.681237813527818),.UNSPECIFIED.);
#453=B_SPLINE_SURFACE_WITH_KNOTS('',3,3,((#23256,#23257,#23258,#23259,#23260),
(#23261,#23262,#23263,#23264,#23265),(#23266,#23267,#23268,#23269,#23270),
(#23271,#23272,#23273,#23274,#23275)),.UNSPECIFIED.,.F.,.F.,.F.,(4,4),(4,
1,4),(0.,1.),(0.,0.571428571428571,1.),.UNSPECIFIED.);
#454=B_SPLINE_SURFACE_WITH_KNOTS('',3,3,((#23419,#23420,#23421,#23422,#23423,
#23424,#23425,#23426,#23427),(#23428,#23429,#23430,#23431,#23432,#23433,
#23434,#23435,#23436),(#23437,#23438,#23439,#23440,#23441,#23442,#23443,
#23444,#23445),(#23446,#23447,#23448,#23449,#23450,#23451,#23452,#23453,
#23454)),.UNSPECIFIED.,.F.,.F.,.F.,(4,4),(4,1,1,1,1,1,4),(0.,1.),(0.,0.214285714285714,
0.357142857142857,0.571428571428571,0.785714285714286,0.857142857142857,
1.),.UNSPECIFIED.);
#455=B_SPLINE_SURFACE_WITH_KNOTS('',3,3,((#23598,#23599,#23600,#23601),
(#23602,#23603,#23604,#23605),(#23606,#23607,#23608,#23609),(#23610,#23611,
#23612,#23613)),.UNSPECIFIED.,.F.,.F.,.F.,(4,4),(4,4),(0.,1.),(9.99629094513149E-5,
0.273153287835104),.UNSPECIFIED.);
#456=B_SPLINE_SURFACE_WITH_KNOTS('',3,3,((#23634,#23635,#23636,#23637),
(#23638,#23639,#23640,#23641),(#23642,#23643,#23644,#23645),(#23646,#23647,
#23648,#23649)),.UNSPECIFIED.,.F.,.F.,.F.,(4,4),(4,4),(0.,1.),(0.273153287835091,
0.310482170393536),.UNSPECIFIED.);
#457=B_SPLINE_SURFACE_WITH_KNOTS('',3,3,((#23658,#23659,#23660,#23661),
(#23662,#23663,#23664,#23665),(#23666,#23667,#23668,#23669),(#23670,#23671,
#23672,#23673)),.UNSPECIFIED.,.F.,.F.,.F.,(4,4),(4,4),(0.,1.),(0.681229980645392,
0.954283455385459),.UNSPECIFIED.);
#458=B_SPLINE_SURFACE_WITH_KNOTS('',3,3,((#23685,#23686,#23687,#23688),
(#23689,#23690,#23691,#23692),(#23693,#23694,#23695,#23696),(#23697,#23698,
#23699,#23700)),.UNSPECIFIED.,.F.,.F.,.F.,(4,4),(4,4),(0.,1.),(0.643901098086959,
0.681229980645406),.UNSPECIFIED.);
#459=B_SPLINE_SURFACE_WITH_KNOTS('',3,3,((#23735,#23736,#23737,#23738,#23739),
(#23740,#23741,#23742,#23743,#23744),(#23745,#23746,#23747,#23748,#23749),
(#23750,#23751,#23752,#23753,#23754)),.UNSPECIFIED.,.F.,.F.,.F.,(4,4),(4,
1,4),(0.,1.),(0.,0.571428571428571,1.),.UNSPECIFIED.);
#460=B_SPLINE_SURFACE_WITH_KNOTS('',3,3,((#23844,#23845,#23846,#23847,#23848,
#23849,#23850,#23851,#23852),(#23853,#23854,#23855,#23856,#23857,#23858,
#23859,#23860,#23861),(#23862,#23863,#23864,#23865,#23866,#23867,#23868,
#23869,#23870),(#23871,#23872,#23873,#23874,#23875,#23876,#23877,#23878,
#23879)),.UNSPECIFIED.,.F.,.F.,.F.,(4,4),(4,1,1,1,1,1,4),(0.,1.),(0.,0.214285714285714,
0.357142857142857,0.571428571428571,0.785714285714286,0.857142857142857,
1.),.UNSPECIFIED.);
#461=B_SPLINE_SURFACE_WITH_KNOTS('',3,3,((#23967,#23968,#23969,#23970),
(#23971,#23972,#23973,#23974),(#23975,#23976,#23977,#23978),(#23979,#23980,
#23981,#23982)),.UNSPECIFIED.,.F.,.F.,.F.,(4,4),(4,4),(0.,1.),(9.9962909451316E-5,
0.273153287835098),.UNSPECIFIED.);
#462=B_SPLINE_SURFACE_WITH_KNOTS('',3,3,((#23995,#23996,#23997,#23998),
(#23999,#24000,#24001,#24002),(#24003,#24004,#24005,#24006),(#24007,#24008,
#24009,#24010)),.UNSPECIFIED.,.F.,.F.,.F.,(4,4),(4,4),(0.,1.),(0.273153287835084,
0.310482170393536),.UNSPECIFIED.);
#463=B_SPLINE_SURFACE_WITH_KNOTS('',3,3,((#24015,#24016,#24017,#24018),
(#24019,#24020,#24021,#24022),(#24023,#24024,#24025,#24026),(#24027,#24028,
#24029,#24030)),.UNSPECIFIED.,.F.,.F.,.F.,(4,4),(4,4),(0.,1.),(0.681229980645393,
0.954283455385461),.UNSPECIFIED.);
#464=B_SPLINE_SURFACE_WITH_KNOTS('',3,3,((#24037,#24038,#24039,#24040),
(#24041,#24042,#24043,#24044),(#24045,#24046,#24047,#24048),(#24049,#24050,
#24051,#24052)),.UNSPECIFIED.,.F.,.F.,.F.,(4,4),(4,4),(0.,1.),(0.64390109808696,
0.681229980645406),.UNSPECIFIED.);
#465=B_SPLINE_SURFACE_WITH_KNOTS('',3,3,((#24154,#24155,#24156,#24157,#24158),
(#24159,#24160,#24161,#24162,#24163),(#24164,#24165,#24166,#24167,#24168),
(#24169,#24170,#24171,#24172,#24173)),.UNSPECIFIED.,.F.,.F.,.F.,(4,4),(4,
1,4),(0.,1.),(0.,0.571428571428571,1.),.UNSPECIFIED.);
#466=B_SPLINE_SURFACE_WITH_KNOTS('',3,3,((#24314,#24315,#24316,#24317,#24318,
#24319,#24320,#24321,#24322),(#24323,#24324,#24325,#24326,#24327,#24328,
#24329,#24330,#24331),(#24332,#24333,#24334,#24335,#24336,#24337,#24338,
#24339,#24340),(#24341,#24342,#24343,#24344,#24345,#24346,#24347,#24348,
#24349)),.UNSPECIFIED.,.F.,.F.,.F.,(4,4),(4,1,1,1,1,1,4),(0.,1.),(0.,0.214285714285714,
0.357142857142857,0.571428571428571,0.785714285714286,0.857142857142857,
1.),.UNSPECIFIED.);
#467=B_SPLINE_SURFACE_WITH_KNOTS('',3,3,((#24407,#24408,#24409,#24410),
(#24411,#24412,#24413,#24414),(#24415,#24416,#24417,#24418),(#24419,#24420,
#24421,#24422)),.UNSPECIFIED.,.F.,.F.,.F.,(4,4),(4,4),(0.,1.),(9.99629094513129E-5,
0.273153287835103),.UNSPECIFIED.);
#468=B_SPLINE_SURFACE_WITH_KNOTS('',3,3,((#24438,#24439,#24440,#24441),
(#24442,#24443,#24444,#24445),(#24446,#24447,#24448,#24449),(#24450,#24451,
#24452,#24453)),.UNSPECIFIED.,.F.,.F.,.F.,(4,4),(4,4),(0.,1.),(0.273153287835089,
0.310482170393537),.UNSPECIFIED.);
#469=B_SPLINE_SURFACE_WITH_KNOTS('',3,3,((#24462,#24463,#24464,#24465),
(#24466,#24467,#24468,#24469),(#24470,#24471,#24472,#24473),(#24474,#24475,
#24476,#24477)),.UNSPECIFIED.,.F.,.F.,.F.,(4,4),(4,4),(0.,1.),(0.681229980645392,
0.95428345538546),.UNSPECIFIED.);
#470=B_SPLINE_SURFACE_WITH_KNOTS('',3,3,((#24489,#24490,#24491,#24492),
(#24493,#24494,#24495,#24496),(#24497,#24498,#24499,#24500),(#24501,#24502,
#24503,#24504)),.UNSPECIFIED.,.F.,.F.,.F.,(4,4),(4,4),(0.,1.),(0.643901098086959,
0.681229980645405),.UNSPECIFIED.);
#471=B_SPLINE_SURFACE_WITH_KNOTS('',3,3,((#24577,#24578,#24579,#24580,#24581,
#24582),(#24583,#24584,#24585,#24586,#24587,#24588),(#24589,#24590,#24591,
#24592,#24593,#24594),(#24595,#24596,#24597,#24598,#24599,#24600)),
 .UNSPECIFIED.,.F.,.F.,.F.,(4,4),(4,1,1,4),(0.,1.),(0.,0.571428571428571,
0.857142857142857,1.),.UNSPECIFIED.);
#472=B_SPLINE_SURFACE_WITH_KNOTS('',3,3,((#24702,#24703,#24704,#24705,#24706,
#24707),(#24708,#24709,#24710,#24711,#24712,#24713),(#24714,#24715,#24716,
#24717,#24718,#24719),(#24720,#24721,#24722,#24723,#24724,#24725)),
 .UNSPECIFIED.,.F.,.F.,.F.,(4,4),(4,1,1,4),(0.,1.),(0.,0.571428571428571,
0.857142857142857,1.),.UNSPECIFIED.);
#473=B_SPLINE_SURFACE_WITH_KNOTS('',3,3,((#24827,#24828,#24829,#24830,#24831,
#24832),(#24833,#24834,#24835,#24836,#24837,#24838),(#24839,#24840,#24841,
#24842,#24843,#24844),(#24845,#24846,#24847,#24848,#24849,#24850)),
 .UNSPECIFIED.,.F.,.F.,.F.,(4,4),(4,1,1,4),(0.,1.),(-1.70953476876622,-0.976877010723551,
-0.48843850536177,1.11854969730985E-14),.UNSPECIFIED.);
#474=B_SPLINE_SURFACE_WITH_KNOTS('',3,3,((#24872,#24873,#24874,#24875,#24876,
#24877,#24878),(#24879,#24880,#24881,#24882,#24883,#24884,#24885),(#24886,
#24887,#24888,#24889,#24890,#24891,#24892),(#24893,#24894,#24895,#24896,
#24897,#24898,#24899)),.UNSPECIFIED.,.F.,.F.,.F.,(4,4),(4,1,1,1,4),(0.,
1.),(-3.1415926535898,-2.77526377456847,-2.40893489554713,-1.92049639018535,
-1.43205788482356),.UNSPECIFIED.);
#475=B_SPLINE_SURFACE_WITH_KNOTS('',3,3,((#25044,#25045,#25046,#25047,#25048,
#25049),(#25050,#25051,#25052,#25053,#25054,#25055),(#25056,#25057,#25058,
#25059,#25060,#25061),(#25062,#25063,#25064,#25065,#25066,#25067)),
 .UNSPECIFIED.,.F.,.F.,.F.,(4,4),(4,1,1,4),(0.,1.),(0.,0.571428571428571,
0.857142857142857,1.),.UNSPECIFIED.);
#476=B_SPLINE_SURFACE_WITH_KNOTS('',3,3,((#25121,#25122,#25123,#25124,#25125,
#25126),(#25127,#25128,#25129,#25130,#25131,#25132),(#25133,#25134,#25135,
#25136,#25137,#25138),(#25139,#25140,#25141,#25142,#25143,#25144)),
 .UNSPECIFIED.,.F.,.F.,.F.,(4,4),(4,1,1,4),(0.,1.),(0.,0.571428571428571,
0.857142857142857,1.),.UNSPECIFIED.);
#477=B_SPLINE_SURFACE_WITH_KNOTS('',3,3,((#25196,#25197,#25198,#25199,#25200,
#25201),(#25202,#25203,#25204,#25205,#25206,#25207),(#25208,#25209,#25210,
#25211,#25212,#25213),(#25214,#25215,#25216,#25217,#25218,#25219)),
 .UNSPECIFIED.,.F.,.F.,.F.,(4,4),(4,1,1,4),(0.,1.),(-1.70953476876624,-0.976877010723567,
-0.488438505361783,0.),.UNSPECIFIED.);
#478=B_SPLINE_SURFACE_WITH_KNOTS('',3,3,((#25232,#25233,#25234,#25235,#25236,
#25237),(#25238,#25239,#25240,#25241,#25242,#25243),(#25244,#25245,#25246,
#25247,#25248,#25249),(#25250,#25251,#25252,#25253,#25254,#25255)),
 .UNSPECIFIED.,.F.,.F.,.F.,(4,4),(4,1,1,4),(0.,1.),(-1.70953476876622,-0.976877010723555,
-0.488438505361777,0.),.UNSPECIFIED.);
#479=B_SPLINE_SURFACE_WITH_KNOTS('',3,3,((#25262,#25263,#25264,#25265,#25266,
#25267),(#25268,#25269,#25270,#25271,#25272,#25273),(#25274,#25275,#25276,
#25277,#25278,#25279),(#25280,#25281,#25282,#25283,#25284,#25285)),
 .UNSPECIFIED.,.F.,.F.,.F.,(4,4),(4,1,1,4),(0.,1.),(0.,0.571428571428571,
0.857142857142857,1.),.UNSPECIFIED.);
#480=B_SPLINE_SURFACE_WITH_KNOTS('',3,3,((#25384,#25385,#25386,#25387,#25388,
#25389),(#25390,#25391,#25392,#25393,#25394,#25395),(#25396,#25397,#25398,
#25399,#25400,#25401),(#25402,#25403,#25404,#25405,#25406,#25407)),
 .UNSPECIFIED.,.F.,.F.,.F.,(4,4),(4,1,1,4),(0.,1.),(0.,0.571428571428571,
0.857142857142857,1.),.UNSPECIFIED.);
#481=B_SPLINE_SURFACE_WITH_KNOTS('',3,3,((#25509,#25510,#25511,#25512,#25513,
#25514),(#25515,#25516,#25517,#25518,#25519,#25520),(#25521,#25522,#25523,
#25524,#25525,#25526),(#25527,#25528,#25529,#25530,#25531,#25532)),
 .UNSPECIFIED.,.F.,.F.,.F.,(4,4),(4,1,1,4),(0.,1.),(-1.70953476876621,-0.976877010723542,
-0.48843850536176,2.22044604925035E-14),.UNSPECIFIED.);
#482=B_SPLINE_SURFACE_WITH_KNOTS('',3,3,((#25554,#25555,#25556,#25557,#25558,
#25559),(#25560,#25561,#25562,#25563,#25564,#25565),(#25566,#25567,#25568,
#25569,#25570,#25571),(#25572,#25573,#25574,#25575,#25576,#25577)),
 .UNSPECIFIED.,.F.,.F.,.F.,(4,4),(4,1,1,4),(0.,1.),(-1.70953476876621,-0.97687701072354,
-0.488438505361759,2.22044604925031E-14),.UNSPECIFIED.);
#483=B_SPLINE_SURFACE_WITH_KNOTS('',3,3,((#25711,#25712,#25713,#25714,#25715,
#25716),(#25717,#25718,#25719,#25720,#25721,#25722),(#25723,#25724,#25725,
#25726,#25727,#25728),(#25729,#25730,#25731,#25732,#25733,#25734)),
 .UNSPECIFIED.,.F.,.F.,.F.,(4,4),(4,1,1,4),(0.,1.),(0.,0.571428571428571,
0.857142857142857,1.),.UNSPECIFIED.);
#484=B_SPLINE_SURFACE_WITH_KNOTS('',3,3,((#25786,#25787,#25788,#25789,#25790,
#25791),(#25792,#25793,#25794,#25795,#25796,#25797),(#25798,#25799,#25800,
#25801,#25802,#25803),(#25804,#25805,#25806,#25807,#25808,#25809)),
 .UNSPECIFIED.,.F.,.F.,.F.,(4,4),(4,1,1,4),(0.,1.),(0.,0.571428571428571,
0.857142857142857,1.),.UNSPECIFIED.);
#485=B_SPLINE_SURFACE_WITH_KNOTS('',3,3,((#25861,#25862,#25863,#25864,#25865,
#25866),(#25867,#25868,#25869,#25870,#25871,#25872),(#25873,#25874,#25875,
#25876,#25877,#25878),(#25879,#25880,#25881,#25882,#25883,#25884)),
 .UNSPECIFIED.,.F.,.F.,.F.,(4,4),(4,1,1,4),(0.,1.),(-1.70953476876623,-0.976877010723562,
-0.488438505361782,-2.77555756156289E-15),.UNSPECIFIED.);
#486=B_SPLINE_SURFACE_WITH_KNOTS('',3,3,((#25897,#25898,#25899,#25900,#25901,
#25902),(#25903,#25904,#25905,#25906,#25907,#25908),(#25909,#25910,#25911,
#25912,#25913,#25914),(#25915,#25916,#25917,#25918,#25919,#25920)),
 .UNSPECIFIED.,.F.,.F.,.F.,(4,4),(4,1,1,4),(0.,1.),(-1.70953476876623,-0.976877010723559,
-0.488438505361781,-2.77555756156289E-15),.UNSPECIFIED.);
#487=B_SPLINE_SURFACE_WITH_KNOTS('',3,3,((#27379,#27380,#27381,#27382,#27383,
#27384,#27385,#27386,#27387,#27388),(#27389,#27390,#27391,#27392,#27393,
#27394,#27395,#27396,#27397,#27398),(#27399,#27400,#27401,#27402,#27403,
#27404,#27405,#27406,#27407,#27408),(#27409,#27410,#27411,#27412,#27413,
#27414,#27415,#27416,#27417,#27418)),.UNSPECIFIED.,.F.,.F.,.F.,(4,4),(4,
1,1,1,1,1,1,4),(0.,1.),(0.,0.0714285714285714,0.142857142857143,0.428571428571429,
0.571428571428571,0.857142857142857,0.928571428571429,1.),.UNSPECIFIED.);
#488=B_SPLINE_SURFACE_WITH_KNOTS('',3,3,((#27589,#27590,#27591,#27592,#27593,
#27594,#27595,#27596,#27597,#27598),(#27599,#27600,#27601,#27602,#27603,
#27604,#27605,#27606,#27607,#27608),(#27609,#27610,#27611,#27612,#27613,
#27614,#27615,#27616,#27617,#27618),(#27619,#27620,#27621,#27622,#27623,
#27624,#27625,#27626,#27627,#27628)),.UNSPECIFIED.,.F.,.F.,.F.,(4,4),(4,
1,1,1,1,1,1,4),(0.,1.),(0.,0.0714285714285714,0.142857142857143,0.428571428571429,
0.571428571428571,0.857142857142857,0.928571428571429,1.),.UNSPECIFIED.);
#489=B_SPLINE_SURFACE_WITH_KNOTS('',3,3,((#27802,#27803,#27804,#27805,#27806),
(#27807,#27808,#27809,#27810,#27811),(#27812,#27813,#27814,#27815,#27816),
(#27817,#27818,#27819,#27820,#27821)),.UNSPECIFIED.,.F.,.F.,.F.,(4,4),(4,
1,4),(0.,1.),(0.000100096646392838,0.202656880902853,0.405213665159313),
 .UNSPECIFIED.);
#490=B_SPLINE_SURFACE_WITH_KNOTS('',3,3,((#27844,#27845,#27846,#27847),
(#27848,#27849,#27850,#27851),(#27852,#27853,#27854,#27855),(#27856,#27857,
#27858,#27859)),.UNSPECIFIED.,.F.,.F.,.F.,(4,4),(4,4),(0.,1.),(0.405213665159311,
0.477037429617388),.UNSPECIFIED.);
#491=B_SPLINE_SURFACE_WITH_KNOTS('',3,3,((#27868,#27869,#27870,#27871,#27872,
#27873,#27874,#27875),(#27876,#27877,#27878,#27879,#27880,#27881,#27882,
#27883),(#27884,#27885,#27886,#27887,#27888,#27889,#27890,#27891),(#27892,
#27893,#27894,#27895,#27896,#27897,#27898,#27899)),.UNSPECIFIED.,.F.,.F.,
 .F.,(4,4),(4,2,2,4),(0.,1.),(1.09363288142463,1.23517682544946,1.36281421029337,
1.49035179973623),.UNSPECIFIED.);
#492=B_SPLINE_SURFACE_WITH_KNOTS('',3,3,((#27919,#27920,#27921,#27922),
(#27923,#27924,#27925,#27926),(#27927,#27928,#27929,#27930),(#27931,#27932,
#27933,#27934)),.UNSPECIFIED.,.F.,.F.,.F.,(4,4),(4,4),(0.,1.),(1.02439235355261,
1.09363288142469),.UNSPECIFIED.);
#493=B_SPLINE_SURFACE_WITH_KNOTS('',3,3,((#28053,#28054,#28055,#28056,#28057,
#28058,#28059,#28060,#28061,#28062),(#28063,#28064,#28065,#28066,#28067,
#28068,#28069,#28070,#28071,#28072),(#28073,#28074,#28075,#28076,#28077,
#28078,#28079,#28080,#28081,#28082),(#28083,#28084,#28085,#28086,#28087,
#28088,#28089,#28090,#28091,#28092)),.UNSPECIFIED.,.F.,.F.,.F.,(4,4),(4,
1,1,1,1,1,1,4),(0.,1.),(0.,0.0714285714285714,0.142857142857143,0.428571428571429,
0.571428571428571,0.857142857142857,0.928571428571429,1.),.UNSPECIFIED.);
#494=B_SPLINE_SURFACE_WITH_KNOTS('',3,3,((#28266,#28267,#28268,#28269,#28270,
#28271,#28272,#28273,#28274,#28275),(#28276,#28277,#28278,#28279,#28280,
#28281,#28282,#28283,#28284,#28285),(#28286,#28287,#28288,#28289,#28290,
#28291,#28292,#28293,#28294,#28295),(#28296,#28297,#28298,#28299,#28300,
#28301,#28302,#28303,#28304,#28305)),.UNSPECIFIED.,.F.,.F.,.F.,(4,4),(4,
1,1,1,1,1,1,4),(0.,1.),(0.,0.0714285714285714,0.142857142857143,0.428571428571429,
0.571428571428571,0.857142857142857,0.928571428571429,1.),.UNSPECIFIED.);
#495=B_SPLINE_SURFACE_WITH_KNOTS('',3,3,((#28479,#28480,#28481,#28482,#28483,
#28484,#28485,#28486),(#28487,#28488,#28489,#28490,#28491,#28492,#28493,
#28494),(#28495,#28496,#28497,#28498,#28499,#28500,#28501,#28502),(#28503,
#28504,#28505,#28506,#28507,#28508,#28509,#28510)),.UNSPECIFIED.,.F.,.F.,
 .F.,(4,4),(4,2,2,4),(0.,1.),(9.99213751786348E-5,0.127637384843918,0.255274769687837,
0.396818713712658),.UNSPECIFIED.);
#496=B_SPLINE_SURFACE_WITH_KNOTS('',3,3,((#28539,#28540,#28541,#28542),
(#28543,#28544,#28545,#28546),(#28547,#28548,#28549,#28550),(#28551,#28552,
#28553,#28554)),.UNSPECIFIED.,.F.,.F.,.F.,(4,4),(4,4),(0.,1.),(0.396818713712602,
0.466059241584687),.UNSPECIFIED.);
#497=B_SPLINE_SURFACE_WITH_KNOTS('',3,3,((#28563,#28564,#28565,#28566,#28567),
(#28568,#28569,#28570,#28571,#28572),(#28573,#28574,#28575,#28576,#28577),
(#28578,#28579,#28580,#28581,#28582)),.UNSPECIFIED.,.F.,.F.,.F.,(4,4),(4,
1,4),(0.,1.),(1.09614424273996,1.29870116660779,1.50125809047561),
 .UNSPECIFIED.);
#498=B_SPLINE_SURFACE_WITH_KNOTS('',3,3,((#28596,#28597,#28598,#28599),
(#28600,#28601,#28602,#28603),(#28604,#28605,#28606,#28607),(#28608,#28609,
#28610,#28611)),.UNSPECIFIED.,.F.,.F.,.F.,(4,4),(4,4),(0.,1.),(1.02432047828189,
1.09614424273996),.UNSPECIFIED.);
#499=B_SPLINE_SURFACE_WITH_KNOTS('',3,3,((#28694,#28695,#28696,#28697,#28698,
#28699,#28700,#28701,#28702,#28703),(#28704,#28705,#28706,#28707,#28708,
#28709,#28710,#28711,#28712,#28713),(#28714,#28715,#28716,#28717,#28718,
#28719,#28720,#28721,#28722,#28723),(#28724,#28725,#28726,#28727,#28728,
#28729,#28730,#28731,#28732,#28733)),.UNSPECIFIED.,.F.,.F.,.F.,(4,4),(4,
1,1,1,1,1,1,4),(0.,1.),(0.,0.0714285714285714,0.142857142857143,0.428571428571429,
0.571428571428571,0.857142857142857,0.928571428571429,1.),.UNSPECIFIED.);
#500=B_SPLINE_SURFACE_WITH_KNOTS('',3,3,((#28836,#28837,#28838,#28839,#28840,
#28841,#28842,#28843,#28844,#28845),(#28846,#28847,#28848,#28849,#28850,
#28851,#28852,#28853,#28854,#28855),(#28856,#28857,#28858,#28859,#28860,
#28861,#28862,#28863,#28864,#28865),(#28866,#28867,#28868,#28869,#28870,
#28871,#28872,#28873,#28874,#28875)),.UNSPECIFIED.,.F.,.F.,.F.,(4,4),(4,
1,1,1,1,1,1,4),(0.,1.),(0.,0.0714285714285714,0.142857142857143,0.428571428571429,
0.571428571428571,0.857142857142857,0.928571428571429,1.),.UNSPECIFIED.);
#501=B_SPLINE_SURFACE_WITH_KNOTS('',3,3,((#28880,#28881,#28882,#28883,#28884,
#28885,#28886),(#28887,#28888,#28889,#28890,#28891,#28892,#28893),(#28894,
#28895,#28896,#28897,#28898,#28899,#28900),(#28901,#28902,#28903,#28904,
#28905,#28906,#28907)),.UNSPECIFIED.,.F.,.F.,.F.,(4,4),(4,2,1,4),(0.,1.),
(9.99213751786565E-5,0.127637384843918,0.289146182165162,0.396818713712658),
 .UNSPECIFIED.);
#502=B_SPLINE_SURFACE_WITH_KNOTS('',3,3,((#28912,#28913,#28914,#28915),
(#28916,#28917,#28918,#28919),(#28920,#28921,#28922,#28923),(#28924,#28925,
#28926,#28927)),.UNSPECIFIED.,.F.,.F.,.F.,(4,4),(4,4),(0.,1.),(0.396818713712603,
0.466059241584687),.UNSPECIFIED.);
#503=B_SPLINE_SURFACE_WITH_KNOTS('',3,3,((#28928,#28929,#28930,#28931,#28932),
(#28933,#28934,#28935,#28936,#28937),(#28938,#28939,#28940,#28941,#28942),
(#28943,#28944,#28945,#28946,#28947)),.UNSPECIFIED.,.F.,.F.,.F.,(4,4),(4,
1,4),(0.,1.),(1.09621611801068,1.29877304187851,1.50132996574633),
 .UNSPECIFIED.);
#504=B_SPLINE_SURFACE_WITH_KNOTS('',3,3,((#28954,#28955,#28956,#28957),
(#28958,#28959,#28960,#28961),(#28962,#28963,#28964,#28965),(#28966,#28967,
#28968,#28969)),.UNSPECIFIED.,.F.,.F.,.F.,(4,4),(4,4),(0.,1.),(1.02439235355261,
1.09621611801068),.UNSPECIFIED.);
#505=B_SPLINE_SURFACE_WITH_KNOTS('',3,3,((#29074,#29075,#29076,#29077,#29078,
#29079,#29080,#29081,#29082,#29083),(#29084,#29085,#29086,#29087,#29088,
#29089,#29090,#29091,#29092,#29093),(#29094,#29095,#29096,#29097,#29098,
#29099,#29100,#29101,#29102,#29103),(#29104,#29105,#29106,#29107,#29108,
#29109,#29110,#29111,#29112,#29113)),.UNSPECIFIED.,.F.,.F.,.F.,(4,4),(4,
1,1,1,1,1,1,4),(0.,1.),(0.,0.0714285714285714,0.142857142857143,0.428571428571429,
0.571428571428571,0.857142857142857,0.928571428571429,1.),.UNSPECIFIED.);
#506=B_SPLINE_SURFACE_WITH_KNOTS('',3,3,((#29218,#29219,#29220,#29221,#29222,
#29223,#29224,#29225,#29226,#29227),(#29228,#29229,#29230,#29231,#29232,
#29233,#29234,#29235,#29236,#29237),(#29238,#29239,#29240,#29241,#29242,
#29243,#29244,#29245,#29246,#29247),(#29248,#29249,#29250,#29251,#29252,
#29253,#29254,#29255,#29256,#29257)),.UNSPECIFIED.,.F.,.F.,.F.,(4,4),(4,
1,1,1,1,1,1,4),(0.,1.),(0.,0.0714285714285714,0.142857142857143,0.428571428571429,
0.571428571428571,0.857142857142857,0.928571428571429,1.),.UNSPECIFIED.);
#507=B_SPLINE_SURFACE_WITH_KNOTS('',3,3,((#29262,#29263,#29264,#29265,#29266),
(#29267,#29268,#29269,#29270,#29271),(#29272,#29273,#29274,#29275,#29276),
(#29277,#29278,#29279,#29280,#29281)),.UNSPECIFIED.,.F.,.F.,.F.,(4,4),(4,
1,4),(0.,1.),(0.000100096646392837,0.202656880902853,0.405213665159313),
 .UNSPECIFIED.);
#508=B_SPLINE_SURFACE_WITH_KNOTS('',3,3,((#29286,#29287,#29288,#29289),
(#29290,#29291,#29292,#29293),(#29294,#29295,#29296,#29297),(#29298,#29299,
#29300,#29301)),.UNSPECIFIED.,.F.,.F.,.F.,(4,4),(4,4),(0.,1.),(0.405213665159311,
0.477037429617386),.UNSPECIFIED.);
#509=B_SPLINE_SURFACE_WITH_KNOTS('',3,3,((#29302,#29303,#29304,#29305,#29306,
#29307),(#29308,#29309,#29310,#29311,#29312,#29313),(#29314,#29315,#29316,
#29317,#29318,#29319),(#29320,#29321,#29322,#29323,#29324,#29325)),
 .UNSPECIFIED.,.F.,.F.,.F.,(4,4),(4,1,1,4),(0.,1.),(1.09363288142463,1.20698114379938,
1.26365527498675,1.49035179973623),.UNSPECIFIED.);
#510=B_SPLINE_SURFACE_WITH_KNOTS('',3,3,((#29333,#29334,#29335,#29336),
(#29337,#29338,#29339,#29340),(#29341,#29342,#29343,#29344),(#29345,#29346,
#29347,#29348)),.UNSPECIFIED.,.F.,.F.,.F.,(4,4),(4,4),(0.,1.),(1.02439235355261,
1.09363288142469),.UNSPECIFIED.);
#511=B_SPLINE_SURFACE_WITH_KNOTS('',3,3,((#29503,#29504,#29505,#29506,#29507,
#29508,#29509,#29510),(#29511,#29512,#29513,#29514,#29515,#29516,#29517,
#29518),(#29519,#29520,#29521,#29522,#29523,#29524,#29525,#29526),(#29527,
#29528,#29529,#29530,#29531,#29532,#29533,#29534)),.UNSPECIFIED.,.F.,.F.,
 .F.,(4,4),(4,1,1,1,1,4),(0.,1.),(0.,0.142857142857143,0.428571428571429,
0.571428571428571,0.857142857142857,1.),.UNSPECIFIED.);
#512=B_SPLINE_SURFACE_WITH_KNOTS('',3,3,((#29708,#29709,#29710,#29711,#29712,
#29713,#29714,#29715),(#29716,#29717,#29718,#29719,#29720,#29721,#29722,
#29723),(#29724,#29725,#29726,#29727,#29728,#29729,#29730,#29731),(#29732,
#29733,#29734,#29735,#29736,#29737,#29738,#29739)),.UNSPECIFIED.,.F.,.F.,
 .F.,(4,4),(4,1,1,1,1,4),(0.,1.),(0.,0.142857142857143,0.428571428571429,
0.571428571428571,0.857142857142857,1.),.UNSPECIFIED.);
#513=B_SPLINE_SURFACE_WITH_KNOTS('',3,3,((#29913,#29914,#29915,#29916,#29917),
(#29918,#29919,#29920,#29921,#29922),(#29923,#29924,#29925,#29926,#29927),
(#29928,#29929,#29930,#29931,#29932)),.UNSPECIFIED.,.F.,.F.,.F.,(4,4),(4,
1,4),(0.,1.),(0.000100085581199305,0.2925237931603,0.511841573844625),
 .UNSPECIFIED.);
#514=B_SPLINE_SURFACE_WITH_KNOTS('',3,3,((#29955,#29956,#29957,#29958),
(#29959,#29960,#29961,#29962),(#29963,#29964,#29965,#29966),(#29967,#29968,
#29969,#29970)),.UNSPECIFIED.,.F.,.F.,.F.,(4,4),(4,4),(0.,1.),(0.511841573844535,
0.568951195767079),.UNSPECIFIED.);
#515=B_SPLINE_SURFACE_WITH_KNOTS('',3,3,((#29979,#29980,#29981,#29982,#29983),
(#29984,#29985,#29986,#29987,#29988),(#29989,#29990,#29991,#29992,#29993),
(#29994,#29995,#29996,#29997,#29998)),.UNSPECIFIED.,.F.,.F.,.F.,(4,4),(4,
1,4),(0.,1.),(1.29126994154665,1.58369377785584,1.80301165508774),
 .UNSPECIFIED.);
#516=B_SPLINE_SURFACE_WITH_KNOTS('',3,3,((#30012,#30013,#30014,#30015),
(#30016,#30017,#30018,#30019),(#30020,#30021,#30022,#30023),(#30024,#30025,
#30026,#30027)),.UNSPECIFIED.,.F.,.F.,.F.,(4,4),(4,4),(0.,1.),(1.2341603196242,
1.29126994154674),.UNSPECIFIED.);
#517=B_SPLINE_SURFACE_WITH_KNOTS('',3,3,((#30153,#30154,#30155,#30156,#30157,
#30158,#30159,#30160,#30161,#30162),(#30163,#30164,#30165,#30166,#30167,
#30168,#30169,#30170,#30171,#30172),(#30173,#30174,#30175,#30176,#30177,
#30178,#30179,#30180,#30181,#30182),(#30183,#30184,#30185,#30186,#30187,
#30188,#30189,#30190,#30191,#30192)),.UNSPECIFIED.,.F.,.F.,.F.,(4,4),(4,
1,1,1,1,1,1,4),(0.,1.),(0.,0.0714285714285714,0.142857142857143,0.428571428571429,
0.571428571428571,0.857142857142857,0.928571428571429,1.),.UNSPECIFIED.);
#518=B_SPLINE_SURFACE_WITH_KNOTS('',3,3,((#30366,#30367,#30368,#30369,#30370,
#30371,#30372,#30373),(#30374,#30375,#30376,#30377,#30378,#30379,#30380,
#30381),(#30382,#30383,#30384,#30385,#30386,#30387,#30388,#30389),(#30390,
#30391,#30392,#30393,#30394,#30395,#30396,#30397)),.UNSPECIFIED.,.F.,.F.,
 .F.,(4,4),(4,1,1,1,1,4),(0.,1.),(0.,0.142857142857143,0.428571428571429,
0.571428571428571,0.857142857142857,1.),.UNSPECIFIED.);
#519=B_SPLINE_SURFACE_WITH_KNOTS('',3,3,((#30473,#30474,#30475,#30476,#30477),
(#30478,#30479,#30480,#30481,#30482),(#30483,#30484,#30485,#30486,#30487),
(#30488,#30489,#30490,#30491,#30492)),.UNSPECIFIED.,.F.,.F.,.F.,(4,4),(4,
1,4),(0.,1.),(0.000100085581199306,0.2925237931603,0.511841573844626),
 .UNSPECIFIED.);
#520=B_SPLINE_SURFACE_WITH_KNOTS('',3,3,((#30509,#30510,#30511,#30512),
(#30513,#30514,#30515,#30516),(#30517,#30518,#30519,#30520),(#30521,#30522,
#30523,#30524)),.UNSPECIFIED.,.F.,.F.,.F.,(4,4),(4,4),(0.,1.),(0.511841573844535,
0.568951195767079),.UNSPECIFIED.);
#521=B_SPLINE_SURFACE_WITH_KNOTS('',3,3,((#30533,#30534,#30535,#30536,#30537),
(#30538,#30539,#30540,#30541,#30542),(#30543,#30544,#30545,#30546,#30547),
(#30548,#30549,#30550,#30551,#30552)),.UNSPECIFIED.,.F.,.F.,.F.,(4,4),(4,
1,4),(0.,1.),(1.30839898923264,1.52771686646454,1.82014070277373),
 .UNSPECIFIED.);
#522=B_SPLINE_SURFACE_WITH_KNOTS('',3,3,((#30566,#30567,#30568,#30569),
(#30570,#30571,#30572,#30573),(#30574,#30575,#30576,#30577),(#30578,#30579,
#30580,#30581)),.UNSPECIFIED.,.F.,.F.,.F.,(4,4),(4,4),(0.,1.),(1.25128936731019,
1.30839898923273),.UNSPECIFIED.);
#523=B_SPLINE_SURFACE_WITH_KNOTS('',3,3,((#30852,#30853,#30854,#30855,#30856,
#30857,#30858,#30859,#30860,#30861),(#30862,#30863,#30864,#30865,#30866,
#30867,#30868,#30869,#30870,#30871),(#30872,#30873,#30874,#30875,#30876,
#30877,#30878,#30879,#30880,#30881),(#30882,#30883,#30884,#30885,#30886,
#30887,#30888,#30889,#30890,#30891)),.UNSPECIFIED.,.F.,.F.,.F.,(4,4),(4,
1,1,1,1,1,1,4),(0.,1.),(0.,0.0714285714285714,0.142857142857143,0.428571428571429,
0.571428571428571,0.857142857142857,0.928571428571429,1.),.UNSPECIFIED.);
#524=B_SPLINE_SURFACE_WITH_KNOTS('',3,3,((#31065,#31066,#31067,#31068,#31069,
#31070,#31071,#31072),(#31073,#31074,#31075,#31076,#31077,#31078,#31079,
#31080),(#31081,#31082,#31083,#31084,#31085,#31086,#31087,#31088),(#31089,
#31090,#31091,#31092,#31093,#31094,#31095,#31096)),.UNSPECIFIED.,.F.,.F.,
 .F.,(4,4),(4,1,1,1,1,4),(0.,1.),(0.,0.142857142857143,0.428571428571429,
0.571428571428571,0.857142857142857,1.),.UNSPECIFIED.);
#525=B_SPLINE_SURFACE_WITH_KNOTS('',3,3,((#31270,#31271,#31272,#31273,#31274),
(#31275,#31276,#31277,#31278,#31279),(#31280,#31281,#31282,#31283,#31284),
(#31285,#31286,#31287,#31288,#31289)),.UNSPECIFIED.,.F.,.F.,.F.,(4,4),(4,
1,4),(0.,1.),(0.000100085581199305,0.2925237931603,0.511841573844626),
 .UNSPECIFIED.);
#526=B_SPLINE_SURFACE_WITH_KNOTS('',3,3,((#31308,#31309,#31310,#31311),
(#31312,#31313,#31314,#31315),(#31316,#31317,#31318,#31319),(#31320,#31321,
#31322,#31323)),.UNSPECIFIED.,.F.,.F.,.F.,(4,4),(4,4),(0.,1.),(0.511841573844536,
0.568951195767079),.UNSPECIFIED.);
#527=B_SPLINE_SURFACE_WITH_KNOTS('',3,3,((#31328,#31329,#31330,#31331,#31332),
(#31333,#31334,#31335,#31336,#31337),(#31338,#31339,#31340,#31341,#31342),
(#31343,#31344,#31345,#31346,#31347)),.UNSPECIFIED.,.F.,.F.,.F.,(4,4),(4,
1,4),(0.,1.),(1.29126994154665,1.58369377785584,1.80301165508774),
 .UNSPECIFIED.);
#528=B_SPLINE_SURFACE_WITH_KNOTS('',3,3,((#31360,#31361,#31362,#31363),
(#31364,#31365,#31366,#31367),(#31368,#31369,#31370,#31371),(#31372,#31373,
#31374,#31375)),.UNSPECIFIED.,.F.,.F.,.F.,(4,4),(4,4),(0.,1.),(1.2341603196242,
1.29126994154674),.UNSPECIFIED.);
#529=B_SPLINE_SURFACE_WITH_KNOTS('',3,3,((#31386,#31387,#31388,#31389,#31390,
#31391,#31392,#31393,#31394,#31395),(#31396,#31397,#31398,#31399,#31400,
#31401,#31402,#31403,#31404,#31405),(#31406,#31407,#31408,#31409,#31410,
#31411,#31412,#31413,#31414,#31415),(#31416,#31417,#31418,#31419,#31420,
#31421,#31422,#31423,#31424,#31425)),.UNSPECIFIED.,.F.,.F.,.F.,(4,4),(4,
1,1,1,1,1,1,4),(0.,1.),(0.,0.0714285714285714,0.142857142857143,0.428571428571429,
0.571428571428571,0.857142857142857,0.928571428571429,1.),.UNSPECIFIED.);
#530=B_SPLINE_SURFACE_WITH_KNOTS('',3,3,((#31527,#31528,#31529,#31530,#31531,
#31532,#31533,#31534),(#31535,#31536,#31537,#31538,#31539,#31540,#31541,
#31542),(#31543,#31544,#31545,#31546,#31547,#31548,#31549,#31550),(#31551,
#31552,#31553,#31554,#31555,#31556,#31557,#31558)),.UNSPECIFIED.,.F.,.F.,
 .F.,(4,4),(4,1,1,1,1,4),(0.,1.),(0.,0.142857142857143,0.428571428571429,
0.571428571428571,0.857142857142857,1.),.UNSPECIFIED.);
#531=B_SPLINE_SURFACE_WITH_KNOTS('',3,3,((#31658,#31659,#31660,#31661,#31662),
(#31663,#31664,#31665,#31666,#31667),(#31668,#31669,#31670,#31671,#31672),
(#31673,#31674,#31675,#31676,#31677)),.UNSPECIFIED.,.F.,.F.,.F.,(4,4),(4,
1,4),(0.,1.),(0.000100085581199306,0.292523793160301,0.511841573844627),
 .UNSPECIFIED.);
#532=B_SPLINE_SURFACE_WITH_KNOTS('',3,3,((#31687,#31688,#31689,#31690),
(#31691,#31692,#31693,#31694),(#31695,#31696,#31697,#31698),(#31699,#31700,
#31701,#31702)),.UNSPECIFIED.,.F.,.F.,.F.,(4,4),(4,4),(0.,1.),(0.511841573844537,
0.568951195767077),.UNSPECIFIED.);
#533=B_SPLINE_SURFACE_WITH_KNOTS('',3,3,((#31703,#31704,#31705,#31706,#31707),
(#31708,#31709,#31710,#31711,#31712),(#31713,#31714,#31715,#31716,#31717),
(#31718,#31719,#31720,#31721,#31722)),.UNSPECIFIED.,.F.,.F.,.F.,(4,4),(4,
1,4),(0.,1.),(1.30839898923264,1.52771686646453,1.82014070277373),
 .UNSPECIFIED.);
#534=B_SPLINE_SURFACE_WITH_KNOTS('',3,3,((#31729,#31730,#31731,#31732),
(#31733,#31734,#31735,#31736),(#31737,#31738,#31739,#31740),(#31741,#31742,
#31743,#31744)),.UNSPECIFIED.,.F.,.F.,.F.,(4,4),(4,4),(0.,1.),(1.25128936731019,
1.30839898923273),.UNSPECIFIED.);
#535=SHAPE_REPRESENTATION_RELATIONSHIP('SRR','None',#32362,#549);
#536=SHAPE_REPRESENTATION_RELATIONSHIP('SRR','None',#32363,#550);
#537=SHAPE_REPRESENTATION_RELATIONSHIP('SRR','None',#32364,#551);
#538=SHAPE_REPRESENTATION_RELATIONSHIP('SRR','None',#32365,#552);
#539=SHAPE_REPRESENTATION_RELATIONSHIP('SRR','None',#32366,#553);
#540=SHAPE_REPRESENTATION_RELATIONSHIP('SRR','None',#32367,#554);
#541=SHAPE_REPRESENTATION_RELATIONSHIP('SRR','None',#32368,#555);
#542=SHAPE_REPRESENTATION_RELATIONSHIP('SRR','None',#32369,#556);
#543=SHAPE_REPRESENTATION_RELATIONSHIP('SRR','None',#32370,#557);
#544=SHAPE_REPRESENTATION_RELATIONSHIP('SRR','None',#32371,#558);
#545=SHAPE_REPRESENTATION_RELATIONSHIP('SRR','None',#32372,#559);
#546=SHAPE_REPRESENTATION_RELATIONSHIP('SRR','None',#32373,#560);
#547=SHAPE_REPRESENTATION_RELATIONSHIP('SRR','None',#32374,#561);
#548=SHAPE_REPRESENTATION_RELATIONSHIP('SRR','None',#32375,#562);
#549=ADVANCED_BREP_SHAPE_REPRESENTATION('',(#577),#32295);
#550=ADVANCED_BREP_SHAPE_REPRESENTATION('',(#578),#32296);
#551=ADVANCED_BREP_SHAPE_REPRESENTATION('',(#579),#32297);
#552=ADVANCED_BREP_SHAPE_REPRESENTATION('',(#580),#32298);
#553=ADVANCED_BREP_SHAPE_REPRESENTATION('',(#581),#32299);
#554=ADVANCED_BREP_SHAPE_REPRESENTATION('',(#582),#32300);
#555=ADVANCED_BREP_SHAPE_REPRESENTATION('',(#583),#32301);
#556=ADVANCED_BREP_SHAPE_REPRESENTATION('',(#584),#32302);
#557=ADVANCED_BREP_SHAPE_REPRESENTATION('',(#585),#32303);
#558=ADVANCED_BREP_SHAPE_REPRESENTATION('',(#586),#32304);
#559=ADVANCED_BREP_SHAPE_REPRESENTATION('',(#587),#32305);
#560=ADVANCED_BREP_SHAPE_REPRESENTATION('',(#588),#32306);
#561=ADVANCED_BREP_SHAPE_REPRESENTATION('',(#589),#32307);
#562=ADVANCED_BREP_SHAPE_REPRESENTATION('',(#590),#32308);
#563=STYLED_ITEM('',(#32488),#577);
#564=STYLED_ITEM('',(#32516),#578);
#565=STYLED_ITEM('',(#32495),#579);
#566=STYLED_ITEM('',(#32516),#580);
#567=STYLED_ITEM('',(#32488),#581);
#568=STYLED_ITEM('',(#32495),#582);
#569=STYLED_ITEM('',(#32495),#583);
#570=STYLED_ITEM('',(#32481),#584);
#571=STYLED_ITEM('',(#32495),#585);
#572=STYLED_ITEM('',(#32502),#586);
#573=STYLED_ITEM('',(#32502),#587);
#574=STYLED_ITEM('',(#32509),#588);
#575=STYLED_ITEM('',(#32495),#589);
#576=STYLED_ITEM('',(#32488),#590);
#577=MANIFOLD_SOLID_BREP('Body1',#13804);
#578=MANIFOLD_SOLID_BREP('Body1',#13805);
#579=MANIFOLD_SOLID_BREP('Body1',#13806);
#580=MANIFOLD_SOLID_BREP('Body1',#13807);
#581=MANIFOLD_SOLID_BREP('Body1',#13808);
#582=MANIFOLD_SOLID_BREP('Body1',#13809);
#583=MANIFOLD_SOLID_BREP('Body1',#13810);
#584=MANIFOLD_SOLID_BREP('Body1',#13811);
#585=MANIFOLD_SOLID_BREP('Body1',#13812);
#586=MANIFOLD_SOLID_BREP('Body1',#13813);
#587=MANIFOLD_SOLID_BREP('Body1',#13814);
#588=MANIFOLD_SOLID_BREP('Body1',#13815);
#589=MANIFOLD_SOLID_BREP('Body1',#13816);
#590=MANIFOLD_SOLID_BREP('Body1',#13817);
#591=FACE_BOUND('',#2051,.T.);
#592=FACE_BOUND('',#2055,.T.);
#593=FACE_BOUND('',#2078,.T.);
#594=FACE_BOUND('',#2095,.T.);
#595=FACE_BOUND('',#2179,.T.);
#596=FACE_BOUND('',#2182,.T.);
#597=FACE_BOUND('',#2196,.T.);
#598=FACE_BOUND('',#2218,.T.);
#599=FACE_BOUND('',#2235,.T.);
#600=FACE_BOUND('',#2236,.T.);
#601=FACE_BOUND('',#2237,.T.);
#602=FACE_BOUND('',#2238,.T.);
#603=FACE_BOUND('',#2239,.T.);
#604=FACE_BOUND('',#2240,.T.);
#605=FACE_BOUND('',#2254,.T.);
#606=FACE_BOUND('',#2255,.T.);
#607=FACE_BOUND('',#2256,.T.);
#608=FACE_BOUND('',#2257,.T.);
#609=FACE_BOUND('',#2258,.T.);
#610=FACE_BOUND('',#2259,.T.);
#611=FACE_BOUND('',#2260,.T.);
#612=FACE_BOUND('',#2273,.T.);
#613=FACE_BOUND('',#2288,.T.);
#614=FACE_BOUND('',#2289,.T.);
#615=FACE_BOUND('',#2290,.T.);
#616=FACE_BOUND('',#2291,.T.);
#617=FACE_BOUND('',#2292,.T.);
#618=FACE_BOUND('',#2293,.T.);
#619=FACE_BOUND('',#2294,.T.);
#620=FACE_BOUND('',#2312,.T.);
#621=FACE_BOUND('',#2313,.T.);
#622=FACE_BOUND('',#2314,.T.);
#623=FACE_BOUND('',#2315,.T.);
#624=FACE_BOUND('',#2316,.T.);
#625=FACE_BOUND('',#2317,.T.);
#626=FACE_BOUND('',#2334,.T.);
#627=FACE_BOUND('',#2435,.T.);
#628=FACE_BOUND('',#2439,.T.);
#629=FACE_BOUND('',#2446,.T.);
#630=FACE_BOUND('',#2488,.T.);
#631=FACE_BOUND('',#2489,.T.);
#632=FACE_BOUND('',#2490,.T.);
#633=FACE_BOUND('',#2491,.T.);
#634=FACE_BOUND('',#2510,.T.);
#635=FACE_BOUND('',#2517,.T.);
#636=FACE_BOUND('',#2524,.T.);
#637=FACE_BOUND('',#2531,.T.);
#638=FACE_BOUND('',#2539,.T.);
#639=FACE_BOUND('',#2543,.T.);
#640=FACE_BOUND('',#2547,.T.);
#641=FACE_BOUND('',#2551,.T.);
#642=FACE_BOUND('',#2638,.T.);
#643=FACE_BOUND('',#2652,.T.);
#644=FACE_BOUND('',#2693,.T.);
#645=FACE_BOUND('',#2804,.T.);
#646=FACE_BOUND('',#2807,.T.);
#647=CYLINDRICAL_SURFACE('',#13991,2.2375);
#648=CYLINDRICAL_SURFACE('',#13995,2.23749999999999);
#649=CYLINDRICAL_SURFACE('',#14015,7.);
#650=CYLINDRICAL_SURFACE('',#14018,7.);
#651=CYLINDRICAL_SURFACE('',#14035,7.);
#652=CYLINDRICAL_SURFACE('',#14051,2.23749999999998);
#653=CYLINDRICAL_SURFACE('',#14052,5.2);
#654=CYLINDRICAL_SURFACE('',#14055,2.2375);
#655=CYLINDRICAL_SURFACE('',#14058,7.);
#656=CYLINDRICAL_SURFACE('',#14064,0.8);
#657=CYLINDRICAL_SURFACE('',#14066,6.00000000000001);
#658=CYLINDRICAL_SURFACE('',#14077,0.8);
#659=CYLINDRICAL_SURFACE('',#14078,6.00000000000001);
#660=CYLINDRICAL_SURFACE('',#14084,0.8);
#661=CYLINDRICAL_SURFACE('',#14085,6.);
#662=CYLINDRICAL_SURFACE('',#14087,0.8);
#663=CYLINDRICAL_SURFACE('',#14088,0.8);
#664=CYLINDRICAL_SURFACE('',#14089,5.99999999999998);
#665=CYLINDRICAL_SURFACE('',#14091,0.8);
#666=CYLINDRICAL_SURFACE('',#14092,0.8);
#667=CYLINDRICAL_SURFACE('',#14094,0.8);
#668=CYLINDRICAL_SURFACE('',#14097,0.8);
#669=CYLINDRICAL_SURFACE('',#14099,0.8);
#670=CYLINDRICAL_SURFACE('',#14102,0.8);
#671=CYLINDRICAL_SURFACE('',#14104,0.8);
#672=CYLINDRICAL_SURFACE('',#14107,0.8);
#673=CYLINDRICAL_SURFACE('',#14109,0.8);
#674=CYLINDRICAL_SURFACE('',#14110,0.8);
#675=CYLINDRICAL_SURFACE('',#14112,0.8);
#676=CYLINDRICAL_SURFACE('',#14118,2.45);
#677=CYLINDRICAL_SURFACE('',#14140,1.30000000000001);
#678=CYLINDRICAL_SURFACE('',#14143,1.30000000000001);
#679=CYLINDRICAL_SURFACE('',#14164,4.50000000000001);
#680=CYLINDRICAL_SURFACE('',#14167,4.50000000000001);
#681=CYLINDRICAL_SURFACE('',#14198,1.3);
#682=CYLINDRICAL_SURFACE('',#14199,1.3);
#683=CYLINDRICAL_SURFACE('',#14201,4.5);
#684=CYLINDRICAL_SURFACE('',#14203,4.5);
#685=CYLINDRICAL_SURFACE('',#14214,5.2);
#686=CYLINDRICAL_SURFACE('',#14218,5.2);
#687=CYLINDRICAL_SURFACE('',#14222,5.2);
#688=CYLINDRICAL_SURFACE('',#14226,5.2);
#689=CYLINDRICAL_SURFACE('',#14230,5.2);
#690=CYLINDRICAL_SURFACE('',#14234,5.2);
#691=CYLINDRICAL_SURFACE('',#14246,5.2);
#692=CYLINDRICAL_SURFACE('',#14264,1.2375);
#693=CYLINDRICAL_SURFACE('',#14266,1.2375);
#694=CYLINDRICAL_SURFACE('',#14275,8.);
#695=CYLINDRICAL_SURFACE('',#14279,5.2);
#696=CYLINDRICAL_SURFACE('',#14283,5.2);
#697=CYLINDRICAL_SURFACE('',#14287,5.2);
#698=CYLINDRICAL_SURFACE('',#14291,5.2);
#699=CYLINDRICAL_SURFACE('',#14295,5.2);
#700=CYLINDRICAL_SURFACE('',#14324,6.00000000000001);
#701=CYLINDRICAL_SURFACE('',#14326,6.00000000000001);
#702=CYLINDRICAL_SURFACE('',#14355,6.00000000000001);
#703=CYLINDRICAL_SURFACE('',#14371,1.2375);
#704=CYLINDRICAL_SURFACE('',#14373,1.23749999999999);
#705=CYLINDRICAL_SURFACE('',#14376,6.00000000000001);
#706=CYLINDRICAL_SURFACE('',#14382,0.8);
#707=CYLINDRICAL_SURFACE('',#14384,6.00000000000001);
#708=CYLINDRICAL_SURFACE('',#14390,0.8);
#709=CYLINDRICAL_SURFACE('',#14396,0.8);
#710=CYLINDRICAL_SURFACE('',#14404,6.00000000000001);
#711=CYLINDRICAL_SURFACE('',#14405,0.8);
#712=CYLINDRICAL_SURFACE('',#14406,0.8);
#713=CYLINDRICAL_SURFACE('',#14407,5.99999999999998);
#714=CYLINDRICAL_SURFACE('',#14408,0.8);
#715=CYLINDRICAL_SURFACE('',#14409,6.);
#716=CYLINDRICAL_SURFACE('',#14411,0.8);
#717=CYLINDRICAL_SURFACE('',#14412,0.8);
#718=CYLINDRICAL_SURFACE('',#14416,0.8);
#719=CYLINDRICAL_SURFACE('',#14418,0.8);
#720=CYLINDRICAL_SURFACE('',#14421,0.8);
#721=CYLINDRICAL_SURFACE('',#14423,0.8);
#722=CYLINDRICAL_SURFACE('',#14426,0.8);
#723=CYLINDRICAL_SURFACE('',#14428,0.8);
#724=CYLINDRICAL_SURFACE('',#14429,0.8);
#725=CYLINDRICAL_SURFACE('',#14431,0.8);
#726=CYLINDRICAL_SURFACE('',#14440,8.99999999999999);
#727=CYLINDRICAL_SURFACE('',#14446,9.);
#728=CYLINDRICAL_SURFACE('',#14458,4.85);
#729=CYLINDRICAL_SURFACE('',#14467,9.);
#730=CYLINDRICAL_SURFACE('',#14473,9.);
#731=CYLINDRICAL_SURFACE('',#14487,2.);
#732=CYLINDRICAL_SURFACE('',#14490,2.);
#733=CYLINDRICAL_SURFACE('',#14502,2.);
#734=CYLINDRICAL_SURFACE('',#14505,2.);
#735=CYLINDRICAL_SURFACE('',#14517,2.);
#736=CYLINDRICAL_SURFACE('',#14581,1.525);
#737=CYLINDRICAL_SURFACE('',#14583,1.525);
#738=CYLINDRICAL_SURFACE('',#14585,1.525);
#739=CYLINDRICAL_SURFACE('',#14587,1.525);
#740=CYLINDRICAL_SURFACE('',#14589,1.525);
#741=CYLINDRICAL_SURFACE('',#14603,2.);
#742=CYLINDRICAL_SURFACE('',#14622,4.75);
#743=CYLINDRICAL_SURFACE('',#14632,1.5);
#744=CYLINDRICAL_SURFACE('',#14707,7.00000000000001);
#745=CYLINDRICAL_SURFACE('',#14710,7.);
#746=CYLINDRICAL_SURFACE('',#14735,9.3);
#747=CYLINDRICAL_SURFACE('',#14737,9.3);
#748=CYLINDRICAL_SURFACE('',#14756,7.00000000000001);
#749=CYLINDRICAL_SURFACE('',#14759,7.00000000000001);
#750=CYLINDRICAL_SURFACE('',#14764,1.5);
#751=CYLINDRICAL_SURFACE('',#14765,7.00000000000001);
#752=CYLINDRICAL_SURFACE('',#14769,1.5);
#753=CYLINDRICAL_SURFACE('',#14771,7.00000000000001);
#754=CYLINDRICAL_SURFACE('',#14790,1.5);
#755=CYLINDRICAL_SURFACE('',#14792,1.5);
#756=CYLINDRICAL_SURFACE('',#14795,7.00000000000001);
#757=CYLINDRICAL_SURFACE('',#14797,7.);
#758=CYLINDRICAL_SURFACE('',#14799,9.30000000000001);
#759=CYLINDRICAL_SURFACE('',#14801,9.30000000000001);
#760=CYLINDRICAL_SURFACE('',#14824,4.50000000000001);
#761=CYLINDRICAL_SURFACE('',#14827,4.5);
#762=CYLINDRICAL_SURFACE('',#14841,2.);
#763=CYLINDRICAL_SURFACE('',#14843,7.00000000000001);
#764=CYLINDRICAL_SURFACE('',#14867,7.00000000000001);
#765=CYLINDRICAL_SURFACE('',#14869,7.00000000000001);
#766=CYLINDRICAL_SURFACE('',#14875,2.);
#767=CYLINDRICAL_SURFACE('',#14877,7.00000000000001);
#768=CYLINDRICAL_SURFACE('',#14879,2.);
#769=CYLINDRICAL_SURFACE('',#14880,2.);
#770=CYLINDRICAL_SURFACE('',#14882,4.50000000000001);
#771=CYLINDRICAL_SURFACE('',#14885,4.50000000000002);
#772=CYLINDRICAL_SURFACE('',#14893,1.6);
#773=CIRCLE('',#13977,2.73749999999998);
#774=CIRCLE('',#13978,2.23749999999999);
#775=CIRCLE('',#13981,2.7375);
#776=CIRCLE('',#13982,2.2375);
#777=CIRCLE('',#13985,2.7375);
#778=CIRCLE('',#13986,2.2375);
#779=CIRCLE('',#13989,2.73749999999998);
#780=CIRCLE('',#13990,2.23749999999998);
#781=CIRCLE('',#13992,2.2375);
#782=CIRCLE('',#13994,5.2);
#783=CIRCLE('',#13996,2.23749999999999);
#784=CIRCLE('',#13999,6.5);
#785=CIRCLE('',#14000,6.5);
#786=CIRCLE('',#14001,6.50000000000001);
#787=CIRCLE('',#14002,6.5);
#788=CIRCLE('',#14005,7.);
#789=CIRCLE('',#14008,7.);
#790=CIRCLE('',#14011,7.);
#791=CIRCLE('',#14014,7.);
#792=CIRCLE('',#14016,7.);
#793=CIRCLE('',#14019,7.);
#794=CIRCLE('',#14023,6.4);
#795=CIRCLE('',#14026,7.);
#796=CIRCLE('',#14027,6.40000000000001);
#797=CIRCLE('',#14030,7.);
#798=CIRCLE('',#14031,6.40000000000001);
#799=CIRCLE('',#14034,6.4);
#800=CIRCLE('',#14037,2.83749999999998);
#801=CIRCLE('',#14038,2.83749999999998);
#802=CIRCLE('',#14039,2.83750000000001);
#803=CIRCLE('',#14040,2.8375);
#804=CIRCLE('',#14045,2.2375);
#805=CIRCLE('',#14048,2.23749999999998);
#806=CIRCLE('',#14053,5.2);
#807=CIRCLE('',#14062,6.00000000000001);
#808=CIRCLE('',#14063,5.80000000000001);
#809=CIRCLE('',#14067,6.00000000000001);
#810=CIRCLE('',#14069,6.00000000000001);
#811=CIRCLE('',#14070,5.80000000000001);
#812=CIRCLE('',#14072,5.99999999999998);
#813=CIRCLE('',#14073,6.);
#814=CIRCLE('',#14075,5.80000000000001);
#815=CIRCLE('',#14076,6.00000000000001);
#816=CIRCLE('',#14080,5.80000000000001);
#817=CIRCLE('',#14082,6.);
#818=CIRCLE('',#14083,5.99999999999998);
#819=CIRCLE('',#14116,2.95);
#820=CIRCLE('',#14117,2.45);
#821=CIRCLE('',#14119,2.45);
#822=CIRCLE('',#14122,2.95);
#823=CIRCLE('',#14126,1.80000000000001);
#824=CIRCLE('',#14127,1.30000000000001);
#825=CIRCLE('',#14130,1.80000000000001);
#826=CIRCLE('',#14131,1.30000000000001);
#827=CIRCLE('',#14134,1.8);
#828=CIRCLE('',#14135,1.3);
#829=CIRCLE('',#14138,1.8);
#830=CIRCLE('',#14139,1.3);
#831=CIRCLE('',#14141,1.30000000000001);
#832=CIRCLE('',#14144,1.30000000000001);
#833=CIRCLE('',#14147,4.00000000000001);
#834=CIRCLE('',#14148,4.00000000000001);
#835=CIRCLE('',#14149,4.);
#836=CIRCLE('',#14150,4.);
#837=CIRCLE('',#14152,4.50000000000001);
#838=CIRCLE('',#14155,4.50000000000001);
#839=CIRCLE('',#14158,4.5);
#840=CIRCLE('',#14161,4.5);
#841=CIRCLE('',#14165,4.50000000000001);
#842=CIRCLE('',#14168,4.50000000000001);
#843=CIRCLE('',#14171,3.90000000000001);
#844=CIRCLE('',#14174,3.90000000000001);
#845=CIRCLE('',#14177,3.9);
#846=CIRCLE('',#14178,4.5);
#847=CIRCLE('',#14181,3.9);
#848=CIRCLE('',#14182,4.5);
#849=CIRCLE('',#14184,1.90000000000001);
#850=CIRCLE('',#14185,1.9);
#851=CIRCLE('',#14186,1.9);
#852=CIRCLE('',#14187,1.90000000000001);
#853=CIRCLE('',#14192,1.3);
#854=CIRCLE('',#14195,1.3);
#855=CIRCLE('',#14206,5.69999999999999);
#856=CIRCLE('',#14207,5.2);
#857=CIRCLE('',#14209,5.7);
#858=CIRCLE('',#14210,5.7);
#859=CIRCLE('',#14211,5.69999999999999);
#860=CIRCLE('',#14212,5.7);
#861=CIRCLE('',#14213,5.7);
#862=CIRCLE('',#14215,5.2);
#863=CIRCLE('',#14217,5.2);
#864=CIRCLE('',#14219,5.2);
#865=CIRCLE('',#14221,5.2);
#866=CIRCLE('',#14223,5.2);
#867=CIRCLE('',#14225,5.2);
#868=CIRCLE('',#14227,5.2);
#869=CIRCLE('',#14229,5.2);
#870=CIRCLE('',#14231,5.2);
#871=CIRCLE('',#14233,5.2);
#872=CIRCLE('',#14235,5.2);
#873=CIRCLE('',#14237,5.69999999999999);
#874=CIRCLE('',#14238,5.2);
#875=CIRCLE('',#14240,5.7);
#876=CIRCLE('',#14241,5.7);
#877=CIRCLE('',#14242,5.69999999999999);
#878=CIRCLE('',#14243,5.7);
#879=CIRCLE('',#14244,5.7);
#880=CIRCLE('',#14245,8.5);
#881=CIRCLE('',#14247,5.2);
#882=CIRCLE('',#14250,1.2375);
#883=CIRCLE('',#14251,1.7375);
#884=CIRCLE('',#14254,1.23749999999999);
#885=CIRCLE('',#14255,1.7375);
#886=CIRCLE('',#14258,1.2375);
#887=CIRCLE('',#14259,1.7375);
#888=CIRCLE('',#14262,1.2375);
#889=CIRCLE('',#14263,1.7375);
#890=CIRCLE('',#14265,1.2375);
#891=CIRCLE('',#14267,1.2375);
#892=CIRCLE('',#14269,5.50000000000001);
#893=CIRCLE('',#14270,5.50000000000001);
#894=CIRCLE('',#14271,5.50000000000002);
#895=CIRCLE('',#14272,5.50000000000002);
#896=CIRCLE('',#14274,8.);
#897=CIRCLE('',#14276,8.);
#898=CIRCLE('',#14278,5.2);
#899=CIRCLE('',#14280,5.2);
#900=CIRCLE('',#14282,5.2);
#901=CIRCLE('',#14284,5.2);
#902=CIRCLE('',#14286,5.2);
#903=CIRCLE('',#14288,5.2);
#904=CIRCLE('',#14290,5.2);
#905=CIRCLE('',#14292,5.2);
#906=CIRCLE('',#14294,5.2);
#907=CIRCLE('',#14296,5.2);
#908=CIRCLE('',#14298,8.5);
#909=CIRCLE('',#14300,5.69999999999999);
#910=CIRCLE('',#14301,5.7);
#911=CIRCLE('',#14302,5.7);
#912=CIRCLE('',#14303,5.69999999999999);
#913=CIRCLE('',#14304,5.7);
#914=CIRCLE('',#14305,5.7);
#915=CIRCLE('',#14314,6.00000000000001);
#916=CIRCLE('',#14317,6.00000000000001);
#917=CIRCLE('',#14320,6.00000000000001);
#918=CIRCLE('',#14323,6.00000000000001);
#919=CIRCLE('',#14325,6.00000000000001);
#920=CIRCLE('',#14327,6.00000000000001);
#921=CIRCLE('',#14329,5.69999999999999);
#922=CIRCLE('',#14330,5.7);
#923=CIRCLE('',#14331,5.7);
#924=CIRCLE('',#14332,5.69999999999999);
#925=CIRCLE('',#14333,5.7);
#926=CIRCLE('',#14334,5.7);
#927=CIRCLE('',#14343,5.40000000000001);
#928=CIRCLE('',#14346,5.40000000000002);
#929=CIRCLE('',#14347,6.00000000000001);
#930=CIRCLE('',#14350,5.40000000000002);
#931=CIRCLE('',#14351,6.00000000000001);
#932=CIRCLE('',#14354,5.40000000000001);
#933=CIRCLE('',#14357,1.8375);
#934=CIRCLE('',#14358,1.8375);
#935=CIRCLE('',#14359,1.83749999999999);
#936=CIRCLE('',#14360,1.8375);
#937=CIRCLE('',#14365,1.2375);
#938=CIRCLE('',#14368,1.23749999999999);
#939=CIRCLE('',#14380,5.80000000000001);
#940=CIRCLE('',#14381,6.00000000000001);
#941=CIRCLE('',#14385,6.00000000000001);
#942=CIRCLE('',#14387,5.80000000000001);
#943=CIRCLE('',#14388,6.00000000000001);
#944=CIRCLE('',#14392,6.);
#945=CIRCLE('',#14393,5.99999999999998);
#946=CIRCLE('',#14395,5.80000000000001);
#947=CIRCLE('',#14399,5.80000000000001);
#948=CIRCLE('',#14400,6.00000000000001);
#949=CIRCLE('',#14402,5.99999999999998);
#950=CIRCLE('',#14403,6.);
#951=CIRCLE('',#14434,9.);
#952=CIRCLE('',#14435,8.5);
#953=CIRCLE('',#14438,8.49999999999999);
#954=CIRCLE('',#14439,8.99999999999999);
#955=CIRCLE('',#14441,8.99999999999999);
#956=CIRCLE('',#14442,8.99999999999999);
#957=CIRCLE('',#14445,1.525);
#958=CIRCLE('',#14448,9.);
#959=CIRCLE('',#14449,9.);
#960=CIRCLE('',#14451,5.35);
#961=CIRCLE('',#14452,4.85);
#962=CIRCLE('',#14454,1.5);
#963=CIRCLE('',#14455,1.5);
#964=CIRCLE('',#14456,1.5);
#965=CIRCLE('',#14457,1.5);
#966=CIRCLE('',#14459,4.85);
#967=CIRCLE('',#14461,9.);
#968=CIRCLE('',#14462,8.5);
#969=CIRCLE('',#14465,8.5);
#970=CIRCLE('',#14466,9.);
#971=CIRCLE('',#14468,9.);
#972=CIRCLE('',#14469,9.);
#973=CIRCLE('',#14472,1.525);
#974=CIRCLE('',#14475,9.);
#975=CIRCLE('',#14476,9.);
#976=CIRCLE('',#14479,1.5);
#977=CIRCLE('',#14480,2.);
#978=CIRCLE('',#14483,1.5);
#979=CIRCLE('',#14484,2.);
#980=CIRCLE('',#14488,2.);
#981=CIRCLE('',#14491,2.);
#982=CIRCLE('',#14495,1.5);
#983=CIRCLE('',#14496,2.);
#984=CIRCLE('',#14499,1.5);
#985=CIRCLE('',#14500,2.);
#986=CIRCLE('',#14503,2.);
#987=CIRCLE('',#14506,2.);
#988=CIRCLE('',#14508,2.);
#989=CIRCLE('',#14515,2.);
#990=CIRCLE('',#14518,2.);
#991=CIRCLE('',#14523,8.49999999999999);
#992=CIRCLE('',#14526,8.5);
#993=CIRCLE('',#14529,8.5);
#994=CIRCLE('',#14532,8.5);
#995=CIRCLE('',#14538,2.);
#996=CIRCLE('',#14539,1.5);
#997=CIRCLE('',#14542,1.5);
#998=CIRCLE('',#14547,1.5);
#999=CIRCLE('',#14550,1.5);
#1000=CIRCLE('',#14559,1.525);
#1001=CIRCLE('',#14566,1.525);
#1002=CIRCLE('',#14573,1.525);
#1003=CIRCLE('',#14580,1.525);
#1004=CIRCLE('',#14582,1.525);
#1005=CIRCLE('',#14584,1.525);
#1006=CIRCLE('',#14586,1.525);
#1007=CIRCLE('',#14588,1.525);
#1008=CIRCLE('',#14612,3.57);
#1009=CIRCLE('',#14613,4.21870057685089);
#1010=CIRCLE('',#14614,4.21870057685089);
#1011=CIRCLE('',#14616,4.48129942314911);
#1012=CIRCLE('',#14617,4.48129942314911);
#1013=CIRCLE('',#14620,4.75);
#1014=CIRCLE('',#14621,4.75);
#1015=CIRCLE('',#14623,4.75);
#1016=CIRCLE('',#14625,4.25);
#1017=CIRCLE('',#14629,1.2);
#1018=CIRCLE('',#14631,1.5);
#1019=CIRCLE('',#14633,1.5);
#1020=CIRCLE('',#14635,1.2);
#1021=CIRCLE('',#14693,7.5);
#1022=CIRCLE('',#14694,7.);
#1023=CIRCLE('',#14697,7.50000000000001);
#1024=CIRCLE('',#14698,7.00000000000001);
#1025=CIRCLE('',#14701,7.50000000000001);
#1026=CIRCLE('',#14702,7.00000000000001);
#1027=CIRCLE('',#14705,7.5);
#1028=CIRCLE('',#14706,7.);
#1029=CIRCLE('',#14708,7.00000000000001);
#1030=CIRCLE('',#14711,7.);
#1031=CIRCLE('',#14714,9.3);
#1032=CIRCLE('',#14715,9.30000000000001);
#1033=CIRCLE('',#14716,9.30000000000001);
#1034=CIRCLE('',#14717,9.3);
#1035=CIRCLE('',#14719,9.8);
#1036=CIRCLE('',#14720,9.3);
#1037=CIRCLE('',#14723,9.8);
#1038=CIRCLE('',#14724,9.3);
#1039=CIRCLE('',#14727,9.80000000000001);
#1040=CIRCLE('',#14728,9.30000000000001);
#1041=CIRCLE('',#14731,9.80000000000001);
#1042=CIRCLE('',#14732,9.30000000000001);
#1043=CIRCLE('',#14739,6.50000000000001);
#1044=CIRCLE('',#14740,6.50000000000001);
#1045=CIRCLE('',#14741,6.50000000000001);
#1046=CIRCLE('',#14742,6.50000000000001);
#1047=CIRCLE('',#14744,7.00000000000001);
#1048=CIRCLE('',#14747,7.00000000000001);
#1049=CIRCLE('',#14750,7.00000000000001);
#1050=CIRCLE('',#14753,7.00000000000001);
#1051=CIRCLE('',#14757,7.00000000000001);
#1052=CIRCLE('',#14760,7.00000000000001);
#1053=CIRCLE('',#14762,6.50000000000001);
#1054=CIRCLE('',#14763,7.00000000000001);
#1055=CIRCLE('',#14767,6.50000000000001);
#1056=CIRCLE('',#14768,7.00000000000001);
#1057=CIRCLE('',#14773,7.50000000000001);
#1058=CIRCLE('',#14776,7.5);
#1059=CIRCLE('',#14779,7.5);
#1060=CIRCLE('',#14780,7.);
#1061=CIRCLE('',#14783,7.50000000000001);
#1062=CIRCLE('',#14784,7.00000000000001);
#1063=CIRCLE('',#14787,6.50000000000001);
#1064=CIRCLE('',#14788,6.50000000000001);
#1065=CIRCLE('',#14805,5.);
#1066=CIRCLE('',#14806,4.5);
#1067=CIRCLE('',#14809,5.00000000000001);
#1068=CIRCLE('',#14810,4.50000000000001);
#1069=CIRCLE('',#14813,5.00000000000002);
#1070=CIRCLE('',#14814,4.50000000000002);
#1071=CIRCLE('',#14817,5.00000000000001);
#1072=CIRCLE('',#14818,4.50000000000001);
#1073=CIRCLE('',#14820,6.50000000000001);
#1074=CIRCLE('',#14821,6.50000000000001);
#1075=CIRCLE('',#14822,6.50000000000001);
#1076=CIRCLE('',#14823,6.50000000000001);
#1077=CIRCLE('',#14825,4.50000000000001);
#1078=CIRCLE('',#14828,4.5);
#1079=CIRCLE('',#14839,7.00000000000001);
#1080=CIRCLE('',#14840,6.50000000000001);
#1081=CIRCLE('',#14844,7.00000000000001);
#1082=CIRCLE('',#14846,7.00000000000001);
#1083=CIRCLE('',#14847,6.50000000000001);
#1084=CIRCLE('',#14849,6.50000000000001);
#1085=CIRCLE('',#14850,6.50000000000001);
#1086=CIRCLE('',#14855,7.00000000000001);
#1087=CIRCLE('',#14858,7.00000000000001);
#1088=CIRCLE('',#14863,7.00000000000001);
#1089=CIRCLE('',#14870,7.00000000000001);
#1090=CIRCLE('',#14874,7.00000000000001);
#1091=CIRCLE('',#14883,4.50000000000001);
#1092=CIRCLE('',#14886,4.50000000000002);
#1093=CIRCLE('',#14891,1.6);
#1094=CIRCLE('',#14892,1.84);
#1095=CIRCLE('',#14894,1.6);
#1096=CIRCLE('',#14897,1.84);
#1097=CONICAL_SURFACE('',#13976,2.48749999999999,0.785398163397441);
#1098=CONICAL_SURFACE('',#13980,2.4875,0.785398163397441);
#1099=CONICAL_SURFACE('',#13984,2.4875,0.785398163397441);
#1100=CONICAL_SURFACE('',#13988,2.48749999999998,0.785398163397441);
#1101=CONICAL_SURFACE('',#14004,6.75,0.785398163397441);
#1102=CONICAL_SURFACE('',#14007,6.75,0.785398163397441);
#1103=CONICAL_SURFACE('',#14010,6.75000000000001,0.785398163397431);
#1104=CONICAL_SURFACE('',#14013,6.75,0.785398163397441);
#1105=CONICAL_SURFACE('',#14022,6.7,0.78539816339745);
#1106=CONICAL_SURFACE('',#14025,6.70000000000001,0.785398163397438);
#1107=CONICAL_SURFACE('',#14029,6.7,0.785398163397445);
#1108=CONICAL_SURFACE('',#14033,6.7,0.78539816339745);
#1109=CONICAL_SURFACE('',#14042,2.5375,0.78539816339745);
#1110=CONICAL_SURFACE('',#14044,2.5375,0.78539816339745);
#1111=CONICAL_SURFACE('',#14047,2.53749999999998,0.785398163397445);
#1112=CONICAL_SURFACE('',#14050,2.53749999999998,0.785398163397445);
#1113=CONICAL_SURFACE('',#14061,5.90000000000001,0.785398163397448);
#1114=CONICAL_SURFACE('',#14068,5.90000000000001,0.785398163397451);
#1115=CONICAL_SURFACE('',#14074,5.90000000000001,0.785398163397451);
#1116=CONICAL_SURFACE('',#14079,5.90000000000001,0.785398163397448);
#1117=CONICAL_SURFACE('',#14115,2.7,0.785398163397451);
#1118=CONICAL_SURFACE('',#14121,2.7,0.785398163397448);
#1119=CONICAL_SURFACE('',#14125,1.55000000000001,0.785398163397447);
#1120=CONICAL_SURFACE('',#14129,1.55000000000001,0.785398163397447);
#1121=CONICAL_SURFACE('',#14133,1.55,0.785398163397449);
#1122=CONICAL_SURFACE('',#14137,1.55,0.785398163397448);
#1123=CONICAL_SURFACE('',#14151,4.25000000000001,0.785398163397448);
#1124=CONICAL_SURFACE('',#14154,4.25000000000001,0.785398163397448);
#1125=CONICAL_SURFACE('',#14157,4.25,0.785398163397448);
#1126=CONICAL_SURFACE('',#14160,4.25,0.785398163397448);
#1127=CONICAL_SURFACE('',#14170,4.20000000000001,0.78539816339745);
#1128=CONICAL_SURFACE('',#14173,4.20000000000001,0.78539816339745);
#1129=CONICAL_SURFACE('',#14176,4.2,0.785398163397449);
#1130=CONICAL_SURFACE('',#14180,4.2,0.785398163397449);
#1131=CONICAL_SURFACE('',#14189,1.60000000000001,0.785398163397449);
#1132=CONICAL_SURFACE('',#14191,1.6,0.785398163397447);
#1133=CONICAL_SURFACE('',#14194,1.6,0.785398163397448);
#1134=CONICAL_SURFACE('',#14197,1.60000000000001,0.78539816339745);
#1135=CONICAL_SURFACE('',#14205,5.44999999999999,0.785398163397448);
#1136=CONICAL_SURFACE('',#14216,5.45,0.785398163397451);
#1137=CONICAL_SURFACE('',#14220,5.45,0.785398163397451);
#1138=CONICAL_SURFACE('',#14224,5.45,0.785398163397448);
#1139=CONICAL_SURFACE('',#14228,5.45,0.785398163397448);
#1140=CONICAL_SURFACE('',#14232,5.44999999999999,0.785398163397448);
#1141=CONICAL_SURFACE('',#14236,5.44999999999999,0.785398163397446);
#1142=CONICAL_SURFACE('',#14249,1.4875,0.785398163397449);
#1143=CONICAL_SURFACE('',#14253,1.48749999999999,0.785398163397452);
#1144=CONICAL_SURFACE('',#14257,1.4875,0.785398163397449);
#1145=CONICAL_SURFACE('',#14261,1.4875,0.785398163397449);
#1146=CONICAL_SURFACE('',#14273,8.25,0.785398163397446);
#1147=CONICAL_SURFACE('',#14277,5.45,0.785398163397446);
#1148=CONICAL_SURFACE('',#14281,5.45,0.785398163397446);
#1149=CONICAL_SURFACE('',#14285,5.45,0.785398163397448);
#1150=CONICAL_SURFACE('',#14289,5.45,0.785398163397448);
#1151=CONICAL_SURFACE('',#14293,5.44999999999999,0.785398163397446);
#1152=CONICAL_SURFACE('',#14297,8.25,0.785398163397446);
#1153=CONICAL_SURFACE('',#14306,5.44999999999999,0.785398163397446);
#1154=CONICAL_SURFACE('',#14307,5.45,0.785398163397446);
#1155=CONICAL_SURFACE('',#14308,5.45,0.785398163397446);
#1156=CONICAL_SURFACE('',#14309,5.45,0.785398163397448);
#1157=CONICAL_SURFACE('',#14310,5.45,0.785398163397448);
#1158=CONICAL_SURFACE('',#14311,5.44999999999999,0.785398163397446);
#1159=CONICAL_SURFACE('',#14313,5.75000000000002,0.785398163397449);
#1160=CONICAL_SURFACE('',#14316,5.75000000000002,0.785398163397449);
#1161=CONICAL_SURFACE('',#14319,5.75000000000001,0.785398163397451);
#1162=CONICAL_SURFACE('',#14322,5.75000000000001,0.785398163397449);
#1163=CONICAL_SURFACE('',#14335,5.44999999999999,0.785398163397448);
#1164=CONICAL_SURFACE('',#14336,5.45,0.785398163397448);
#1165=CONICAL_SURFACE('',#14337,5.45,0.785398163397448);
#1166=CONICAL_SURFACE('',#14338,5.45,0.785398163397451);
#1167=CONICAL_SURFACE('',#14339,5.45,0.785398163397451);
#1168=CONICAL_SURFACE('',#14340,5.44999999999999,0.785398163397448);
#1169=CONICAL_SURFACE('',#14342,5.70000000000001,0.785398163397431);
#1170=CONICAL_SURFACE('',#14345,5.70000000000002,0.785398163397426);
#1171=CONICAL_SURFACE('',#14349,5.70000000000002,0.785398163397426);
#1172=CONICAL_SURFACE('',#14353,5.70000000000001,0.785398163397431);
#1173=CONICAL_SURFACE('',#14362,1.5375,0.78539816339743);
#1174=CONICAL_SURFACE('',#14364,1.5375,0.78539816339743);
#1175=CONICAL_SURFACE('',#14367,1.53749999999999,0.785398163397429);
#1176=CONICAL_SURFACE('',#14370,1.5375,0.785398163397426);
#1177=CONICAL_SURFACE('',#14379,5.90000000000001,0.785398163397448);
#1178=CONICAL_SURFACE('',#14386,5.90000000000001,0.785398163397451);
#1179=CONICAL_SURFACE('',#14394,5.90000000000001,0.785398163397448);
#1180=CONICAL_SURFACE('',#14398,5.90000000000001,0.785398163397451);
#1181=CONICAL_SURFACE('',#14433,8.75,0.785398163397444);
#1182=CONICAL_SURFACE('',#14437,8.75,0.785398163397449);
#1183=CONICAL_SURFACE('',#14450,5.1,0.785398163397447);
#1184=CONICAL_SURFACE('',#14460,8.75,0.785398163397449);
#1185=CONICAL_SURFACE('',#14464,8.75,0.785398163397451);
#1186=CONICAL_SURFACE('',#14478,1.75,0.785398163397449);
#1187=CONICAL_SURFACE('',#14482,1.75,0.785398163397449);
#1188=CONICAL_SURFACE('',#14494,1.75,0.785398163397449);
#1189=CONICAL_SURFACE('',#14498,1.75,0.785398163397449);
#1190=CONICAL_SURFACE('',#14507,1.75,0.785398163397447);
#1191=CONICAL_SURFACE('',#14510,1.75,0.785398163397447);
#1192=CONICAL_SURFACE('',#14512,1.75,0.785398163397447);
#1193=CONICAL_SURFACE('',#14514,1.75,0.785398163397447);
#1194=CONICAL_SURFACE('',#14522,8.75,0.785398163397449);
#1195=CONICAL_SURFACE('',#14525,8.75,0.785398163397449);
#1196=CONICAL_SURFACE('',#14528,8.75,0.785398163397449);
#1197=CONICAL_SURFACE('',#14531,8.75,0.785398163397449);
#1198=CONICAL_SURFACE('',#14537,1.75,0.785398163397447);
#1199=CONICAL_SURFACE('',#14541,1.75,0.785398163397447);
#1200=CONICAL_SURFACE('',#14546,1.75,0.785398163397447);
#1201=CONICAL_SURFACE('',#14549,1.75,0.785398163397447);
#1202=CONICAL_SURFACE('',#14611,3.89435028842544,1.17809724509617);
#1203=CONICAL_SURFACE('',#14615,4.35,0.785398163397448);
#1204=CONICAL_SURFACE('',#14619,4.61564971157455,0.39269908169873);
#1205=CONICAL_SURFACE('',#14626,4.5,0.896055384571344);
#1206=CONICAL_SURFACE('',#14630,1.35,0.785398163397448);
#1207=CONICAL_SURFACE('',#14634,1.35,0.785398163397451);
#1208=CONICAL_SURFACE('',#14692,7.25,0.785398163397452);
#1209=CONICAL_SURFACE('',#14696,7.25000000000001,0.785398163397451);
#1210=CONICAL_SURFACE('',#14700,7.25000000000001,0.785398163397451);
#1211=CONICAL_SURFACE('',#14704,7.25,0.785398163397452);
#1212=CONICAL_SURFACE('',#14718,9.55,0.785398163397451);
#1213=CONICAL_SURFACE('',#14722,9.55,0.785398163397449);
#1214=CONICAL_SURFACE('',#14726,9.55,0.785398163397449);
#1215=CONICAL_SURFACE('',#14730,9.55000000000001,0.785398163397449);
#1216=CONICAL_SURFACE('',#14743,6.75000000000001,0.785398163397449);
#1217=CONICAL_SURFACE('',#14746,6.75000000000001,0.785398163397449);
#1218=CONICAL_SURFACE('',#14749,6.75000000000001,0.785398163397451);
#1219=CONICAL_SURFACE('',#14752,6.75000000000001,0.785398163397449);
#1220=CONICAL_SURFACE('',#14761,6.75000000000001,0.785398163397451);
#1221=CONICAL_SURFACE('',#14766,6.75000000000001,0.785398163397449);
#1222=CONICAL_SURFACE('',#14772,7.25000000000001,0.785398163397451);
#1223=CONICAL_SURFACE('',#14775,7.25,0.785398163397452);
#1224=CONICAL_SURFACE('',#14778,7.25,0.785398163397452);
#1225=CONICAL_SURFACE('',#14782,7.25000000000001,0.785398163397451);
#1226=CONICAL_SURFACE('',#14789,6.75000000000001,0.785398163397449);
#1227=CONICAL_SURFACE('',#14791,6.75000000000001,0.785398163397449);
#1228=CONICAL_SURFACE('',#14804,4.75,0.785398163397449);
#1229=CONICAL_SURFACE('',#14808,4.75000000000001,0.785398163397451);
#1230=CONICAL_SURFACE('',#14812,4.75000000000002,0.785398163397449);
#1231=CONICAL_SURFACE('',#14816,4.75000000000001,0.785398163397449);
#1232=CONICAL_SURFACE('',#14838,6.75000000000001,0.785398163397441);
#1233=CONICAL_SURFACE('',#14845,6.75000000000001,0.785398163397444);
#1234=CONICAL_SURFACE('',#14854,6.75000000000001,0.785398163397449);
#1235=CONICAL_SURFACE('',#14857,6.75000000000001,0.785398163397449);
#1236=CONICAL_SURFACE('',#14860,6.75000000000001,0.785398163397449);
#1237=CONICAL_SURFACE('',#14862,6.75000000000001,0.785398163397449);
#1238=CONICAL_SURFACE('',#14873,6.75000000000001,0.785398163397441);
#1239=CONICAL_SURFACE('',#14878,6.75000000000001,0.785398163397441);
#1240=CONICAL_SURFACE('',#14890,1.72,0.785398163397448);
#1241=CONICAL_SURFACE('',#14896,1.72,0.785398163397448);
#1242=FACE_OUTER_BOUND('',#2041,.T.);
#1243=FACE_OUTER_BOUND('',#2042,.T.);
#1244=FACE_OUTER_BOUND('',#2043,.T.);
#1245=FACE_OUTER_BOUND('',#2044,.T.);
#1246=FACE_OUTER_BOUND('',#2045,.T.);
#1247=FACE_OUTER_BOUND('',#2046,.T.);
#1248=FACE_OUTER_BOUND('',#2047,.T.);
#1249=FACE_OUTER_BOUND('',#2048,.T.);
#1250=FACE_OUTER_BOUND('',#2049,.T.);
#1251=FACE_OUTER_BOUND('',#2050,.T.);
#1252=FACE_OUTER_BOUND('',#2052,.T.);
#1253=FACE_OUTER_BOUND('',#2053,.T.);
#1254=FACE_OUTER_BOUND('',#2054,.T.);
#1255=FACE_OUTER_BOUND('',#2056,.T.);
#1256=FACE_OUTER_BOUND('',#2057,.T.);
#1257=FACE_OUTER_BOUND('',#2058,.T.);
#1258=FACE_OUTER_BOUND('',#2059,.T.);
#1259=FACE_OUTER_BOUND('',#2060,.T.);
#1260=FACE_OUTER_BOUND('',#2061,.T.);
#1261=FACE_OUTER_BOUND('',#2062,.T.);
#1262=FACE_OUTER_BOUND('',#2063,.T.);
#1263=FACE_OUTER_BOUND('',#2064,.T.);
#1264=FACE_OUTER_BOUND('',#2065,.T.);
#1265=FACE_OUTER_BOUND('',#2066,.T.);
#1266=FACE_OUTER_BOUND('',#2067,.T.);
#1267=FACE_OUTER_BOUND('',#2068,.T.);
#1268=FACE_OUTER_BOUND('',#2069,.T.);
#1269=FACE_OUTER_BOUND('',#2070,.T.);
#1270=FACE_OUTER_BOUND('',#2071,.T.);
#1271=FACE_OUTER_BOUND('',#2072,.T.);
#1272=FACE_OUTER_BOUND('',#2073,.T.);
#1273=FACE_OUTER_BOUND('',#2074,.T.);
#1274=FACE_OUTER_BOUND('',#2075,.T.);
#1275=FACE_OUTER_BOUND('',#2076,.T.);
#1276=FACE_OUTER_BOUND('',#2077,.T.);
#1277=FACE_OUTER_BOUND('',#2079,.T.);
#1278=FACE_OUTER_BOUND('',#2080,.T.);
#1279=FACE_OUTER_BOUND('',#2081,.T.);
#1280=FACE_OUTER_BOUND('',#2082,.T.);
#1281=FACE_OUTER_BOUND('',#2083,.T.);
#1282=FACE_OUTER_BOUND('',#2084,.T.);
#1283=FACE_OUTER_BOUND('',#2085,.T.);
#1284=FACE_OUTER_BOUND('',#2086,.T.);
#1285=FACE_OUTER_BOUND('',#2087,.T.);
#1286=FACE_OUTER_BOUND('',#2088,.T.);
#1287=FACE_OUTER_BOUND('',#2089,.T.);
#1288=FACE_OUTER_BOUND('',#2090,.T.);
#1289=FACE_OUTER_BOUND('',#2091,.T.);
#1290=FACE_OUTER_BOUND('',#2092,.T.);
#1291=FACE_OUTER_BOUND('',#2093,.T.);
#1292=FACE_OUTER_BOUND('',#2094,.T.);
#1293=FACE_OUTER_BOUND('',#2096,.T.);
#1294=FACE_OUTER_BOUND('',#2097,.T.);
#1295=FACE_OUTER_BOUND('',#2098,.T.);
#1296=FACE_OUTER_BOUND('',#2099,.T.);
#1297=FACE_OUTER_BOUND('',#2100,.T.);
#1298=FACE_OUTER_BOUND('',#2101,.T.);
#1299=FACE_OUTER_BOUND('',#2102,.T.);
#1300=FACE_OUTER_BOUND('',#2103,.T.);
#1301=FACE_OUTER_BOUND('',#2104,.T.);
#1302=FACE_OUTER_BOUND('',#2105,.T.);
#1303=FACE_OUTER_BOUND('',#2106,.T.);
#1304=FACE_OUTER_BOUND('',#2107,.T.);
#1305=FACE_OUTER_BOUND('',#2108,.T.);
#1306=FACE_OUTER_BOUND('',#2109,.T.);
#1307=FACE_OUTER_BOUND('',#2110,.T.);
#1308=FACE_OUTER_BOUND('',#2111,.T.);
#1309=FACE_OUTER_BOUND('',#2112,.T.);
#1310=FACE_OUTER_BOUND('',#2113,.T.);
#1311=FACE_OUTER_BOUND('',#2114,.T.);
#1312=FACE_OUTER_BOUND('',#2115,.T.);
#1313=FACE_OUTER_BOUND('',#2116,.T.);
#1314=FACE_OUTER_BOUND('',#2117,.T.);
#1315=FACE_OUTER_BOUND('',#2118,.T.);
#1316=FACE_OUTER_BOUND('',#2119,.T.);
#1317=FACE_OUTER_BOUND('',#2120,.T.);
#1318=FACE_OUTER_BOUND('',#2121,.T.);
#1319=FACE_OUTER_BOUND('',#2122,.T.);
#1320=FACE_OUTER_BOUND('',#2123,.T.);
#1321=FACE_OUTER_BOUND('',#2124,.T.);
#1322=FACE_OUTER_BOUND('',#2125,.T.);
#1323=FACE_OUTER_BOUND('',#2126,.T.);
#1324=FACE_OUTER_BOUND('',#2127,.T.);
#1325=FACE_OUTER_BOUND('',#2128,.T.);
#1326=FACE_OUTER_BOUND('',#2129,.T.);
#1327=FACE_OUTER_BOUND('',#2130,.T.);
#1328=FACE_OUTER_BOUND('',#2131,.T.);
#1329=FACE_OUTER_BOUND('',#2132,.T.);
#1330=FACE_OUTER_BOUND('',#2133,.T.);
#1331=FACE_OUTER_BOUND('',#2134,.T.);
#1332=FACE_OUTER_BOUND('',#2135,.T.);
#1333=FACE_OUTER_BOUND('',#2136,.T.);
#1334=FACE_OUTER_BOUND('',#2137,.T.);
#1335=FACE_OUTER_BOUND('',#2138,.T.);
#1336=FACE_OUTER_BOUND('',#2139,.T.);
#1337=FACE_OUTER_BOUND('',#2140,.T.);
#1338=FACE_OUTER_BOUND('',#2141,.T.);
#1339=FACE_OUTER_BOUND('',#2142,.T.);
#1340=FACE_OUTER_BOUND('',#2143,.T.);
#1341=FACE_OUTER_BOUND('',#2144,.T.);
#1342=FACE_OUTER_BOUND('',#2145,.T.);
#1343=FACE_OUTER_BOUND('',#2146,.T.);
#1344=FACE_OUTER_BOUND('',#2147,.T.);
#1345=FACE_OUTER_BOUND('',#2148,.T.);
#1346=FACE_OUTER_BOUND('',#2149,.T.);
#1347=FACE_OUTER_BOUND('',#2150,.T.);
#1348=FACE_OUTER_BOUND('',#2151,.T.);
#1349=FACE_OUTER_BOUND('',#2152,.T.);
#1350=FACE_OUTER_BOUND('',#2153,.T.);
#1351=FACE_OUTER_BOUND('',#2154,.T.);
#1352=FACE_OUTER_BOUND('',#2155,.T.);
#1353=FACE_OUTER_BOUND('',#2156,.T.);
#1354=FACE_OUTER_BOUND('',#2157,.T.);
#1355=FACE_OUTER_BOUND('',#2158,.T.);
#1356=FACE_OUTER_BOUND('',#2159,.T.);
#1357=FACE_OUTER_BOUND('',#2160,.T.);
#1358=FACE_OUTER_BOUND('',#2161,.T.);
#1359=FACE_OUTER_BOUND('',#2162,.T.);
#1360=FACE_OUTER_BOUND('',#2163,.T.);
#1361=FACE_OUTER_BOUND('',#2164,.T.);
#1362=FACE_OUTER_BOUND('',#2165,.T.);
#1363=FACE_OUTER_BOUND('',#2166,.T.);
#1364=FACE_OUTER_BOUND('',#2167,.T.);
#1365=FACE_OUTER_BOUND('',#2168,.T.);
#1366=FACE_OUTER_BOUND('',#2169,.T.);
#1367=FACE_OUTER_BOUND('',#2170,.T.);
#1368=FACE_OUTER_BOUND('',#2171,.T.);
#1369=FACE_OUTER_BOUND('',#2172,.T.);
#1370=FACE_OUTER_BOUND('',#2173,.T.);
#1371=FACE_OUTER_BOUND('',#2174,.T.);
#1372=FACE_OUTER_BOUND('',#2175,.T.);
#1373=FACE_OUTER_BOUND('',#2176,.T.);
#1374=FACE_OUTER_BOUND('',#2177,.T.);
#1375=FACE_OUTER_BOUND('',#2178,.T.);
#1376=FACE_OUTER_BOUND('',#2180,.T.);
#1377=FACE_OUTER_BOUND('',#2181,.T.);
#1378=FACE_OUTER_BOUND('',#2183,.T.);
#1379=FACE_OUTER_BOUND('',#2184,.T.);
#1380=FACE_OUTER_BOUND('',#2185,.T.);
#1381=FACE_OUTER_BOUND('',#2186,.T.);
#1382=FACE_OUTER_BOUND('',#2187,.T.);
#1383=FACE_OUTER_BOUND('',#2188,.T.);
#1384=FACE_OUTER_BOUND('',#2189,.T.);
#1385=FACE_OUTER_BOUND('',#2190,.T.);
#1386=FACE_OUTER_BOUND('',#2191,.T.);
#1387=FACE_OUTER_BOUND('',#2192,.T.);
#1388=FACE_OUTER_BOUND('',#2193,.T.);
#1389=FACE_OUTER_BOUND('',#2194,.T.);
#1390=FACE_OUTER_BOUND('',#2195,.T.);
#1391=FACE_OUTER_BOUND('',#2197,.T.);
#1392=FACE_OUTER_BOUND('',#2198,.T.);
#1393=FACE_OUTER_BOUND('',#2199,.T.);
#1394=FACE_OUTER_BOUND('',#2200,.T.);
#1395=FACE_OUTER_BOUND('',#2201,.T.);
#1396=FACE_OUTER_BOUND('',#2202,.T.);
#1397=FACE_OUTER_BOUND('',#2203,.T.);
#1398=FACE_OUTER_BOUND('',#2204,.T.);
#1399=FACE_OUTER_BOUND('',#2205,.T.);
#1400=FACE_OUTER_BOUND('',#2206,.T.);
#1401=FACE_OUTER_BOUND('',#2207,.T.);
#1402=FACE_OUTER_BOUND('',#2208,.T.);
#1403=FACE_OUTER_BOUND('',#2209,.T.);
#1404=FACE_OUTER_BOUND('',#2210,.T.);
#1405=FACE_OUTER_BOUND('',#2211,.T.);
#1406=FACE_OUTER_BOUND('',#2212,.T.);
#1407=FACE_OUTER_BOUND('',#2213,.T.);
#1408=FACE_OUTER_BOUND('',#2214,.T.);
#1409=FACE_OUTER_BOUND('',#2215,.T.);
#1410=FACE_OUTER_BOUND('',#2216,.T.);
#1411=FACE_OUTER_BOUND('',#2217,.T.);
#1412=FACE_OUTER_BOUND('',#2219,.T.);
#1413=FACE_OUTER_BOUND('',#2220,.T.);
#1414=FACE_OUTER_BOUND('',#2221,.T.);
#1415=FACE_OUTER_BOUND('',#2222,.T.);
#1416=FACE_OUTER_BOUND('',#2223,.T.);
#1417=FACE_OUTER_BOUND('',#2224,.T.);
#1418=FACE_OUTER_BOUND('',#2225,.T.);
#1419=FACE_OUTER_BOUND('',#2226,.T.);
#1420=FACE_OUTER_BOUND('',#2227,.T.);
#1421=FACE_OUTER_BOUND('',#2228,.T.);
#1422=FACE_OUTER_BOUND('',#2229,.T.);
#1423=FACE_OUTER_BOUND('',#2230,.T.);
#1424=FACE_OUTER_BOUND('',#2231,.T.);
#1425=FACE_OUTER_BOUND('',#2232,.T.);
#1426=FACE_OUTER_BOUND('',#2233,.T.);
#1427=FACE_OUTER_BOUND('',#2234,.T.);
#1428=FACE_OUTER_BOUND('',#2241,.T.);
#1429=FACE_OUTER_BOUND('',#2242,.T.);
#1430=FACE_OUTER_BOUND('',#2243,.T.);
#1431=FACE_OUTER_BOUND('',#2244,.T.);
#1432=FACE_OUTER_BOUND('',#2245,.T.);
#1433=FACE_OUTER_BOUND('',#2246,.T.);
#1434=FACE_OUTER_BOUND('',#2247,.T.);
#1435=FACE_OUTER_BOUND('',#2248,.T.);
#1436=FACE_OUTER_BOUND('',#2249,.T.);
#1437=FACE_OUTER_BOUND('',#2250,.T.);
#1438=FACE_OUTER_BOUND('',#2251,.T.);
#1439=FACE_OUTER_BOUND('',#2252,.T.);
#1440=FACE_OUTER_BOUND('',#2253,.T.);
#1441=FACE_OUTER_BOUND('',#2261,.T.);
#1442=FACE_OUTER_BOUND('',#2262,.T.);
#1443=FACE_OUTER_BOUND('',#2263,.T.);
#1444=FACE_OUTER_BOUND('',#2264,.T.);
#1445=FACE_OUTER_BOUND('',#2265,.T.);
#1446=FACE_OUTER_BOUND('',#2266,.T.);
#1447=FACE_OUTER_BOUND('',#2267,.T.);
#1448=FACE_OUTER_BOUND('',#2268,.T.);
#1449=FACE_OUTER_BOUND('',#2269,.T.);
#1450=FACE_OUTER_BOUND('',#2270,.T.);
#1451=FACE_OUTER_BOUND('',#2271,.T.);
#1452=FACE_OUTER_BOUND('',#2272,.T.);
#1453=FACE_OUTER_BOUND('',#2274,.T.);
#1454=FACE_OUTER_BOUND('',#2275,.T.);
#1455=FACE_OUTER_BOUND('',#2276,.T.);
#1456=FACE_OUTER_BOUND('',#2277,.T.);
#1457=FACE_OUTER_BOUND('',#2278,.T.);
#1458=FACE_OUTER_BOUND('',#2279,.T.);
#1459=FACE_OUTER_BOUND('',#2280,.T.);
#1460=FACE_OUTER_BOUND('',#2281,.T.);
#1461=FACE_OUTER_BOUND('',#2282,.T.);
#1462=FACE_OUTER_BOUND('',#2283,.T.);
#1463=FACE_OUTER_BOUND('',#2284,.T.);
#1464=FACE_OUTER_BOUND('',#2285,.T.);
#1465=FACE_OUTER_BOUND('',#2286,.T.);
#1466=FACE_OUTER_BOUND('',#2287,.T.);
#1467=FACE_OUTER_BOUND('',#2295,.T.);
#1468=FACE_OUTER_BOUND('',#2296,.T.);
#1469=FACE_OUTER_BOUND('',#2297,.T.);
#1470=FACE_OUTER_BOUND('',#2298,.T.);
#1471=FACE_OUTER_BOUND('',#2299,.T.);
#1472=FACE_OUTER_BOUND('',#2300,.T.);
#1473=FACE_OUTER_BOUND('',#2301,.T.);
#1474=FACE_OUTER_BOUND('',#2302,.T.);
#1475=FACE_OUTER_BOUND('',#2303,.T.);
#1476=FACE_OUTER_BOUND('',#2304,.T.);
#1477=FACE_OUTER_BOUND('',#2305,.T.);
#1478=FACE_OUTER_BOUND('',#2306,.T.);
#1479=FACE_OUTER_BOUND('',#2307,.T.);
#1480=FACE_OUTER_BOUND('',#2308,.T.);
#1481=FACE_OUTER_BOUND('',#2309,.T.);
#1482=FACE_OUTER_BOUND('',#2310,.T.);
#1483=FACE_OUTER_BOUND('',#2311,.T.);
#1484=FACE_OUTER_BOUND('',#2318,.T.);
#1485=FACE_OUTER_BOUND('',#2319,.T.);
#1486=FACE_OUTER_BOUND('',#2320,.T.);
#1487=FACE_OUTER_BOUND('',#2321,.T.);
#1488=FACE_OUTER_BOUND('',#2322,.T.);
#1489=FACE_OUTER_BOUND('',#2323,.T.);
#1490=FACE_OUTER_BOUND('',#2324,.T.);
#1491=FACE_OUTER_BOUND('',#2325,.T.);
#1492=FACE_OUTER_BOUND('',#2326,.T.);
#1493=FACE_OUTER_BOUND('',#2327,.T.);
#1494=FACE_OUTER_BOUND('',#2328,.T.);
#1495=FACE_OUTER_BOUND('',#2329,.T.);
#1496=FACE_OUTER_BOUND('',#2330,.T.);
#1497=FACE_OUTER_BOUND('',#2331,.T.);
#1498=FACE_OUTER_BOUND('',#2332,.T.);
#1499=FACE_OUTER_BOUND('',#2333,.T.);
#1500=FACE_OUTER_BOUND('',#2335,.T.);
#1501=FACE_OUTER_BOUND('',#2336,.T.);
#1502=FACE_OUTER_BOUND('',#2337,.T.);
#1503=FACE_OUTER_BOUND('',#2338,.T.);
#1504=FACE_OUTER_BOUND('',#2339,.T.);
#1505=FACE_OUTER_BOUND('',#2340,.T.);
#1506=FACE_OUTER_BOUND('',#2341,.T.);
#1507=FACE_OUTER_BOUND('',#2342,.T.);
#1508=FACE_OUTER_BOUND('',#2343,.T.);
#1509=FACE_OUTER_BOUND('',#2344,.T.);
#1510=FACE_OUTER_BOUND('',#2345,.T.);
#1511=FACE_OUTER_BOUND('',#2346,.T.);
#1512=FACE_OUTER_BOUND('',#2347,.T.);
#1513=FACE_OUTER_BOUND('',#2348,.T.);
#1514=FACE_OUTER_BOUND('',#2349,.T.);
#1515=FACE_OUTER_BOUND('',#2350,.T.);
#1516=FACE_OUTER_BOUND('',#2351,.T.);
#1517=FACE_OUTER_BOUND('',#2352,.T.);
#1518=FACE_OUTER_BOUND('',#2353,.T.);
#1519=FACE_OUTER_BOUND('',#2354,.T.);
#1520=FACE_OUTER_BOUND('',#2355,.T.);
#1521=FACE_OUTER_BOUND('',#2356,.T.);
#1522=FACE_OUTER_BOUND('',#2357,.T.);
#1523=FACE_OUTER_BOUND('',#2358,.T.);
#1524=FACE_OUTER_BOUND('',#2359,.T.);
#1525=FACE_OUTER_BOUND('',#2360,.T.);
#1526=FACE_OUTER_BOUND('',#2361,.T.);
#1527=FACE_OUTER_BOUND('',#2362,.T.);
#1528=FACE_OUTER_BOUND('',#2363,.T.);
#1529=FACE_OUTER_BOUND('',#2364,.T.);
#1530=FACE_OUTER_BOUND('',#2365,.T.);
#1531=FACE_OUTER_BOUND('',#2366,.T.);
#1532=FACE_OUTER_BOUND('',#2367,.T.);
#1533=FACE_OUTER_BOUND('',#2368,.T.);
#1534=FACE_OUTER_BOUND('',#2369,.T.);
#1535=FACE_OUTER_BOUND('',#2370,.T.);
#1536=FACE_OUTER_BOUND('',#2371,.T.);
#1537=FACE_OUTER_BOUND('',#2372,.T.);
#1538=FACE_OUTER_BOUND('',#2373,.T.);
#1539=FACE_OUTER_BOUND('',#2374,.T.);
#1540=FACE_OUTER_BOUND('',#2375,.T.);
#1541=FACE_OUTER_BOUND('',#2376,.T.);
#1542=FACE_OUTER_BOUND('',#2377,.T.);
#1543=FACE_OUTER_BOUND('',#2378,.T.);
#1544=FACE_OUTER_BOUND('',#2379,.T.);
#1545=FACE_OUTER_BOUND('',#2380,.T.);
#1546=FACE_OUTER_BOUND('',#2381,.T.);
#1547=FACE_OUTER_BOUND('',#2382,.T.);
#1548=FACE_OUTER_BOUND('',#2383,.T.);
#1549=FACE_OUTER_BOUND('',#2384,.T.);
#1550=FACE_OUTER_BOUND('',#2385,.T.);
#1551=FACE_OUTER_BOUND('',#2386,.T.);
#1552=FACE_OUTER_BOUND('',#2387,.T.);
#1553=FACE_OUTER_BOUND('',#2388,.T.);
#1554=FACE_OUTER_BOUND('',#2389,.T.);
#1555=FACE_OUTER_BOUND('',#2390,.T.);
#1556=FACE_OUTER_BOUND('',#2391,.T.);
#1557=FACE_OUTER_BOUND('',#2392,.T.);
#1558=FACE_OUTER_BOUND('',#2393,.T.);
#1559=FACE_OUTER_BOUND('',#2394,.T.);
#1560=FACE_OUTER_BOUND('',#2395,.T.);
#1561=FACE_OUTER_BOUND('',#2396,.T.);
#1562=FACE_OUTER_BOUND('',#2397,.T.);
#1563=FACE_OUTER_BOUND('',#2398,.T.);
#1564=FACE_OUTER_BOUND('',#2399,.T.);
#1565=FACE_OUTER_BOUND('',#2400,.T.);
#1566=FACE_OUTER_BOUND('',#2401,.T.);
#1567=FACE_OUTER_BOUND('',#2402,.T.);
#1568=FACE_OUTER_BOUND('',#2403,.T.);
#1569=FACE_OUTER_BOUND('',#2404,.T.);
#1570=FACE_OUTER_BOUND('',#2405,.T.);
#1571=FACE_OUTER_BOUND('',#2406,.T.);
#1572=FACE_OUTER_BOUND('',#2407,.T.);
#1573=FACE_OUTER_BOUND('',#2408,.T.);
#1574=FACE_OUTER_BOUND('',#2409,.T.);
#1575=FACE_OUTER_BOUND('',#2410,.T.);
#1576=FACE_OUTER_BOUND('',#2411,.T.);
#1577=FACE_OUTER_BOUND('',#2412,.T.);
#1578=FACE_OUTER_BOUND('',#2413,.T.);
#1579=FACE_OUTER_BOUND('',#2414,.T.);
#1580=FACE_OUTER_BOUND('',#2415,.T.);
#1581=FACE_OUTER_BOUND('',#2416,.T.);
#1582=FACE_OUTER_BOUND('',#2417,.T.);
#1583=FACE_OUTER_BOUND('',#2418,.T.);
#1584=FACE_OUTER_BOUND('',#2419,.T.);
#1585=FACE_OUTER_BOUND('',#2420,.T.);
#1586=FACE_OUTER_BOUND('',#2421,.T.);
#1587=FACE_OUTER_BOUND('',#2422,.T.);
#1588=FACE_OUTER_BOUND('',#2423,.T.);
#1589=FACE_OUTER_BOUND('',#2424,.T.);
#1590=FACE_OUTER_BOUND('',#2425,.T.);
#1591=FACE_OUTER_BOUND('',#2426,.T.);
#1592=FACE_OUTER_BOUND('',#2427,.T.);
#1593=FACE_OUTER_BOUND('',#2428,.T.);
#1594=FACE_OUTER_BOUND('',#2429,.T.);
#1595=FACE_OUTER_BOUND('',#2430,.T.);
#1596=FACE_OUTER_BOUND('',#2431,.T.);
#1597=FACE_OUTER_BOUND('',#2432,.T.);
#1598=FACE_OUTER_BOUND('',#2433,.T.);
#1599=FACE_OUTER_BOUND('',#2434,.T.);
#1600=FACE_OUTER_BOUND('',#2436,.T.);
#1601=FACE_OUTER_BOUND('',#2437,.T.);
#1602=FACE_OUTER_BOUND('',#2438,.T.);
#1603=FACE_OUTER_BOUND('',#2440,.T.);
#1604=FACE_OUTER_BOUND('',#2441,.T.);
#1605=FACE_OUTER_BOUND('',#2442,.T.);
#1606=FACE_OUTER_BOUND('',#2443,.T.);
#1607=FACE_OUTER_BOUND('',#2444,.T.);
#1608=FACE_OUTER_BOUND('',#2445,.T.);
#1609=FACE_OUTER_BOUND('',#2447,.T.);
#1610=FACE_OUTER_BOUND('',#2448,.T.);
#1611=FACE_OUTER_BOUND('',#2449,.T.);
#1612=FACE_OUTER_BOUND('',#2450,.T.);
#1613=FACE_OUTER_BOUND('',#2451,.T.);
#1614=FACE_OUTER_BOUND('',#2452,.T.);
#1615=FACE_OUTER_BOUND('',#2453,.T.);
#1616=FACE_OUTER_BOUND('',#2454,.T.);
#1617=FACE_OUTER_BOUND('',#2455,.T.);
#1618=FACE_OUTER_BOUND('',#2456,.T.);
#1619=FACE_OUTER_BOUND('',#2457,.T.);
#1620=FACE_OUTER_BOUND('',#2458,.T.);
#1621=FACE_OUTER_BOUND('',#2459,.T.);
#1622=FACE_OUTER_BOUND('',#2460,.T.);
#1623=FACE_OUTER_BOUND('',#2461,.T.);
#1624=FACE_OUTER_BOUND('',#2462,.T.);
#1625=FACE_OUTER_BOUND('',#2463,.T.);
#1626=FACE_OUTER_BOUND('',#2464,.T.);
#1627=FACE_OUTER_BOUND('',#2465,.T.);
#1628=FACE_OUTER_BOUND('',#2466,.T.);
#1629=FACE_OUTER_BOUND('',#2467,.T.);
#1630=FACE_OUTER_BOUND('',#2468,.T.);
#1631=FACE_OUTER_BOUND('',#2469,.T.);
#1632=FACE_OUTER_BOUND('',#2470,.T.);
#1633=FACE_OUTER_BOUND('',#2471,.T.);
#1634=FACE_OUTER_BOUND('',#2472,.T.);
#1635=FACE_OUTER_BOUND('',#2473,.T.);
#1636=FACE_OUTER_BOUND('',#2474,.T.);
#1637=FACE_OUTER_BOUND('',#2475,.T.);
#1638=FACE_OUTER_BOUND('',#2476,.T.);
#1639=FACE_OUTER_BOUND('',#2477,.T.);
#1640=FACE_OUTER_BOUND('',#2478,.T.);
#1641=FACE_OUTER_BOUND('',#2479,.T.);
#1642=FACE_OUTER_BOUND('',#2480,.T.);
#1643=FACE_OUTER_BOUND('',#2481,.T.);
#1644=FACE_OUTER_BOUND('',#2482,.T.);
#1645=FACE_OUTER_BOUND('',#2483,.T.);
#1646=FACE_OUTER_BOUND('',#2484,.T.);
#1647=FACE_OUTER_BOUND('',#2485,.T.);
#1648=FACE_OUTER_BOUND('',#2486,.T.);
#1649=FACE_OUTER_BOUND('',#2487,.T.);
#1650=FACE_OUTER_BOUND('',#2492,.T.);
#1651=FACE_OUTER_BOUND('',#2493,.T.);
#1652=FACE_OUTER_BOUND('',#2494,.T.);
#1653=FACE_OUTER_BOUND('',#2495,.T.);
#1654=FACE_OUTER_BOUND('',#2496,.T.);
#1655=FACE_OUTER_BOUND('',#2497,.T.);
#1656=FACE_OUTER_BOUND('',#2498,.T.);
#1657=FACE_OUTER_BOUND('',#2499,.T.);
#1658=FACE_OUTER_BOUND('',#2500,.T.);
#1659=FACE_OUTER_BOUND('',#2501,.T.);
#1660=FACE_OUTER_BOUND('',#2502,.T.);
#1661=FACE_OUTER_BOUND('',#2503,.T.);
#1662=FACE_OUTER_BOUND('',#2504,.T.);
#1663=FACE_OUTER_BOUND('',#2505,.T.);
#1664=FACE_OUTER_BOUND('',#2506,.T.);
#1665=FACE_OUTER_BOUND('',#2507,.T.);
#1666=FACE_OUTER_BOUND('',#2508,.T.);
#1667=FACE_OUTER_BOUND('',#2509,.T.);
#1668=FACE_OUTER_BOUND('',#2511,.T.);
#1669=FACE_OUTER_BOUND('',#2512,.T.);
#1670=FACE_OUTER_BOUND('',#2513,.T.);
#1671=FACE_OUTER_BOUND('',#2514,.T.);
#1672=FACE_OUTER_BOUND('',#2515,.T.);
#1673=FACE_OUTER_BOUND('',#2516,.T.);
#1674=FACE_OUTER_BOUND('',#2518,.T.);
#1675=FACE_OUTER_BOUND('',#2519,.T.);
#1676=FACE_OUTER_BOUND('',#2520,.T.);
#1677=FACE_OUTER_BOUND('',#2521,.T.);
#1678=FACE_OUTER_BOUND('',#2522,.T.);
#1679=FACE_OUTER_BOUND('',#2523,.T.);
#1680=FACE_OUTER_BOUND('',#2525,.T.);
#1681=FACE_OUTER_BOUND('',#2526,.T.);
#1682=FACE_OUTER_BOUND('',#2527,.T.);
#1683=FACE_OUTER_BOUND('',#2528,.T.);
#1684=FACE_OUTER_BOUND('',#2529,.T.);
#1685=FACE_OUTER_BOUND('',#2530,.T.);
#1686=FACE_OUTER_BOUND('',#2532,.T.);
#1687=FACE_OUTER_BOUND('',#2533,.T.);
#1688=FACE_OUTER_BOUND('',#2534,.T.);
#1689=FACE_OUTER_BOUND('',#2535,.T.);
#1690=FACE_OUTER_BOUND('',#2536,.T.);
#1691=FACE_OUTER_BOUND('',#2537,.T.);
#1692=FACE_OUTER_BOUND('',#2538,.T.);
#1693=FACE_OUTER_BOUND('',#2540,.T.);
#1694=FACE_OUTER_BOUND('',#2541,.T.);
#1695=FACE_OUTER_BOUND('',#2542,.T.);
#1696=FACE_OUTER_BOUND('',#2544,.T.);
#1697=FACE_OUTER_BOUND('',#2545,.T.);
#1698=FACE_OUTER_BOUND('',#2546,.T.);
#1699=FACE_OUTER_BOUND('',#2548,.T.);
#1700=FACE_OUTER_BOUND('',#2549,.T.);
#1701=FACE_OUTER_BOUND('',#2550,.T.);
#1702=FACE_OUTER_BOUND('',#2552,.T.);
#1703=FACE_OUTER_BOUND('',#2553,.T.);
#1704=FACE_OUTER_BOUND('',#2554,.T.);
#1705=FACE_OUTER_BOUND('',#2555,.T.);
#1706=FACE_OUTER_BOUND('',#2556,.T.);
#1707=FACE_OUTER_BOUND('',#2557,.T.);
#1708=FACE_OUTER_BOUND('',#2558,.T.);
#1709=FACE_OUTER_BOUND('',#2559,.T.);
#1710=FACE_OUTER_BOUND('',#2560,.T.);
#1711=FACE_OUTER_BOUND('',#2561,.T.);
#1712=FACE_OUTER_BOUND('',#2562,.T.);
#1713=FACE_OUTER_BOUND('',#2563,.T.);
#1714=FACE_OUTER_BOUND('',#2564,.T.);
#1715=FACE_OUTER_BOUND('',#2565,.T.);
#1716=FACE_OUTER_BOUND('',#2566,.T.);
#1717=FACE_OUTER_BOUND('',#2567,.T.);
#1718=FACE_OUTER_BOUND('',#2568,.T.);
#1719=FACE_OUTER_BOUND('',#2569,.T.);
#1720=FACE_OUTER_BOUND('',#2570,.T.);
#1721=FACE_OUTER_BOUND('',#2571,.T.);
#1722=FACE_OUTER_BOUND('',#2572,.T.);
#1723=FACE_OUTER_BOUND('',#2573,.T.);
#1724=FACE_OUTER_BOUND('',#2574,.T.);
#1725=FACE_OUTER_BOUND('',#2575,.T.);
#1726=FACE_OUTER_BOUND('',#2576,.T.);
#1727=FACE_OUTER_BOUND('',#2577,.T.);
#1728=FACE_OUTER_BOUND('',#2578,.T.);
#1729=FACE_OUTER_BOUND('',#2579,.T.);
#1730=FACE_OUTER_BOUND('',#2580,.T.);
#1731=FACE_OUTER_BOUND('',#2581,.T.);
#1732=FACE_OUTER_BOUND('',#2582,.T.);
#1733=FACE_OUTER_BOUND('',#2583,.T.);
#1734=FACE_OUTER_BOUND('',#2584,.T.);
#1735=FACE_OUTER_BOUND('',#2585,.T.);
#1736=FACE_OUTER_BOUND('',#2586,.T.);
#1737=FACE_OUTER_BOUND('',#2587,.T.);
#1738=FACE_OUTER_BOUND('',#2588,.T.);
#1739=FACE_OUTER_BOUND('',#2589,.T.);
#1740=FACE_OUTER_BOUND('',#2590,.T.);
#1741=FACE_OUTER_BOUND('',#2591,.T.);
#1742=FACE_OUTER_BOUND('',#2592,.T.);
#1743=FACE_OUTER_BOUND('',#2593,.T.);
#1744=FACE_OUTER_BOUND('',#2594,.T.);
#1745=FACE_OUTER_BOUND('',#2595,.T.);
#1746=FACE_OUTER_BOUND('',#2596,.T.);
#1747=FACE_OUTER_BOUND('',#2597,.T.);
#1748=FACE_OUTER_BOUND('',#2598,.T.);
#1749=FACE_OUTER_BOUND('',#2599,.T.);
#1750=FACE_OUTER_BOUND('',#2600,.T.);
#1751=FACE_OUTER_BOUND('',#2601,.T.);
#1752=FACE_OUTER_BOUND('',#2602,.T.);
#1753=FACE_OUTER_BOUND('',#2603,.T.);
#1754=FACE_OUTER_BOUND('',#2604,.T.);
#1755=FACE_OUTER_BOUND('',#2605,.T.);
#1756=FACE_OUTER_BOUND('',#2606,.T.);
#1757=FACE_OUTER_BOUND('',#2607,.T.);
#1758=FACE_OUTER_BOUND('',#2608,.T.);
#1759=FACE_OUTER_BOUND('',#2609,.T.);
#1760=FACE_OUTER_BOUND('',#2610,.T.);
#1761=FACE_OUTER_BOUND('',#2611,.T.);
#1762=FACE_OUTER_BOUND('',#2612,.T.);
#1763=FACE_OUTER_BOUND('',#2613,.T.);
#1764=FACE_OUTER_BOUND('',#2614,.T.);
#1765=FACE_OUTER_BOUND('',#2615,.T.);
#1766=FACE_OUTER_BOUND('',#2616,.T.);
#1767=FACE_OUTER_BOUND('',#2617,.T.);
#1768=FACE_OUTER_BOUND('',#2618,.T.);
#1769=FACE_OUTER_BOUND('',#2619,.T.);
#1770=FACE_OUTER_BOUND('',#2620,.T.);
#1771=FACE_OUTER_BOUND('',#2621,.T.);
#1772=FACE_OUTER_BOUND('',#2622,.T.);
#1773=FACE_OUTER_BOUND('',#2623,.T.);
#1774=FACE_OUTER_BOUND('',#2624,.T.);
#1775=FACE_OUTER_BOUND('',#2625,.T.);
#1776=FACE_OUTER_BOUND('',#2626,.T.);
#1777=FACE_OUTER_BOUND('',#2627,.T.);
#1778=FACE_OUTER_BOUND('',#2628,.T.);
#1779=FACE_OUTER_BOUND('',#2629,.T.);
#1780=FACE_OUTER_BOUND('',#2630,.T.);
#1781=FACE_OUTER_BOUND('',#2631,.T.);
#1782=FACE_OUTER_BOUND('',#2632,.T.);
#1783=FACE_OUTER_BOUND('',#2633,.T.);
#1784=FACE_OUTER_BOUND('',#2634,.T.);
#1785=FACE_OUTER_BOUND('',#2635,.T.);
#1786=FACE_OUTER_BOUND('',#2636,.T.);
#1787=FACE_OUTER_BOUND('',#2637,.T.);
#1788=FACE_OUTER_BOUND('',#2639,.T.);
#1789=FACE_OUTER_BOUND('',#2640,.T.);
#1790=FACE_OUTER_BOUND('',#2641,.T.);
#1791=FACE_OUTER_BOUND('',#2642,.T.);
#1792=FACE_OUTER_BOUND('',#2643,.T.);
#1793=FACE_OUTER_BOUND('',#2644,.T.);
#1794=FACE_OUTER_BOUND('',#2645,.T.);
#1795=FACE_OUTER_BOUND('',#2646,.T.);
#1796=FACE_OUTER_BOUND('',#2647,.T.);
#1797=FACE_OUTER_BOUND('',#2648,.T.);
#1798=FACE_OUTER_BOUND('',#2649,.T.);
#1799=FACE_OUTER_BOUND('',#2650,.T.);
#1800=FACE_OUTER_BOUND('',#2651,.T.);
#1801=FACE_OUTER_BOUND('',#2653,.T.);
#1802=FACE_OUTER_BOUND('',#2654,.T.);
#1803=FACE_OUTER_BOUND('',#2655,.T.);
#1804=FACE_OUTER_BOUND('',#2656,.T.);
#1805=FACE_OUTER_BOUND('',#2657,.T.);
#1806=FACE_OUTER_BOUND('',#2658,.T.);
#1807=FACE_OUTER_BOUND('',#2659,.T.);
#1808=FACE_OUTER_BOUND('',#2660,.T.);
#1809=FACE_OUTER_BOUND('',#2661,.T.);
#1810=FACE_OUTER_BOUND('',#2662,.T.);
#1811=FACE_OUTER_BOUND('',#2663,.T.);
#1812=FACE_OUTER_BOUND('',#2664,.T.);
#1813=FACE_OUTER_BOUND('',#2665,.T.);
#1814=FACE_OUTER_BOUND('',#2666,.T.);
#1815=FACE_OUTER_BOUND('',#2667,.T.);
#1816=FACE_OUTER_BOUND('',#2668,.T.);
#1817=FACE_OUTER_BOUND('',#2669,.T.);
#1818=FACE_OUTER_BOUND('',#2670,.T.);
#1819=FACE_OUTER_BOUND('',#2671,.T.);
#1820=FACE_OUTER_BOUND('',#2672,.T.);
#1821=FACE_OUTER_BOUND('',#2673,.T.);
#1822=FACE_OUTER_BOUND('',#2674,.T.);
#1823=FACE_OUTER_BOUND('',#2675,.T.);
#1824=FACE_OUTER_BOUND('',#2676,.T.);
#1825=FACE_OUTER_BOUND('',#2677,.T.);
#1826=FACE_OUTER_BOUND('',#2678,.T.);
#1827=FACE_OUTER_BOUND('',#2679,.T.);
#1828=FACE_OUTER_BOUND('',#2680,.T.);
#1829=FACE_OUTER_BOUND('',#2681,.T.);
#1830=FACE_OUTER_BOUND('',#2682,.T.);
#1831=FACE_OUTER_BOUND('',#2683,.T.);
#1832=FACE_OUTER_BOUND('',#2684,.T.);
#1833=FACE_OUTER_BOUND('',#2685,.T.);
#1834=FACE_OUTER_BOUND('',#2686,.T.);
#1835=FACE_OUTER_BOUND('',#2687,.T.);
#1836=FACE_OUTER_BOUND('',#2688,.T.);
#1837=FACE_OUTER_BOUND('',#2689,.T.);
#1838=FACE_OUTER_BOUND('',#2690,.T.);
#1839=FACE_OUTER_BOUND('',#2691,.T.);
#1840=FACE_OUTER_BOUND('',#2692,.T.);
#1841=FACE_OUTER_BOUND('',#2694,.T.);
#1842=FACE_OUTER_BOUND('',#2695,.T.);
#1843=FACE_OUTER_BOUND('',#2696,.T.);
#1844=FACE_OUTER_BOUND('',#2697,.T.);
#1845=FACE_OUTER_BOUND('',#2698,.T.);
#1846=FACE_OUTER_BOUND('',#2699,.T.);
#1847=FACE_OUTER_BOUND('',#2700,.T.);
#1848=FACE_OUTER_BOUND('',#2701,.T.);
#1849=FACE_OUTER_BOUND('',#2702,.T.);
#1850=FACE_OUTER_BOUND('',#2703,.T.);
#1851=FACE_OUTER_BOUND('',#2704,.T.);
#1852=FACE_OUTER_BOUND('',#2705,.T.);
#1853=FACE_OUTER_BOUND('',#2706,.T.);
#1854=FACE_OUTER_BOUND('',#2707,.T.);
#1855=FACE_OUTER_BOUND('',#2708,.T.);
#1856=FACE_OUTER_BOUND('',#2709,.T.);
#1857=FACE_OUTER_BOUND('',#2710,.T.);
#1858=FACE_OUTER_BOUND('',#2711,.T.);
#1859=FACE_OUTER_BOUND('',#2712,.T.);
#1860=FACE_OUTER_BOUND('',#2713,.T.);
#1861=FACE_OUTER_BOUND('',#2714,.T.);
#1862=FACE_OUTER_BOUND('',#2715,.T.);
#1863=FACE_OUTER_BOUND('',#2716,.T.);
#1864=FACE_OUTER_BOUND('',#2717,.T.);
#1865=FACE_OUTER_BOUND('',#2718,.T.);
#1866=FACE_OUTER_BOUND('',#2719,.T.);
#1867=FACE_OUTER_BOUND('',#2720,.T.);
#1868=FACE_OUTER_BOUND('',#2721,.T.);
#1869=FACE_OUTER_BOUND('',#2722,.T.);
#1870=FACE_OUTER_BOUND('',#2723,.T.);
#1871=FACE_OUTER_BOUND('',#2724,.T.);
#1872=FACE_OUTER_BOUND('',#2725,.T.);
#1873=FACE_OUTER_BOUND('',#2726,.T.);
#1874=FACE_OUTER_BOUND('',#2727,.T.);
#1875=FACE_OUTER_BOUND('',#2728,.T.);
#1876=FACE_OUTER_BOUND('',#2729,.T.);
#1877=FACE_OUTER_BOUND('',#2730,.T.);
#1878=FACE_OUTER_BOUND('',#2731,.T.);
#1879=FACE_OUTER_BOUND('',#2732,.T.);
#1880=FACE_OUTER_BOUND('',#2733,.T.);
#1881=FACE_OUTER_BOUND('',#2734,.T.);
#1882=FACE_OUTER_BOUND('',#2735,.T.);
#1883=FACE_OUTER_BOUND('',#2736,.T.);
#1884=FACE_OUTER_BOUND('',#2737,.T.);
#1885=FACE_OUTER_BOUND('',#2738,.T.);
#1886=FACE_OUTER_BOUND('',#2739,.T.);
#1887=FACE_OUTER_BOUND('',#2740,.T.);
#1888=FACE_OUTER_BOUND('',#2741,.T.);
#1889=FACE_OUTER_BOUND('',#2742,.T.);
#1890=FACE_OUTER_BOUND('',#2743,.T.);
#1891=FACE_OUTER_BOUND('',#2744,.T.);
#1892=FACE_OUTER_BOUND('',#2745,.T.);
#1893=FACE_OUTER_BOUND('',#2746,.T.);
#1894=FACE_OUTER_BOUND('',#2747,.T.);
#1895=FACE_OUTER_BOUND('',#2748,.T.);
#1896=FACE_OUTER_BOUND('',#2749,.T.);
#1897=FACE_OUTER_BOUND('',#2750,.T.);
#1898=FACE_OUTER_BOUND('',#2751,.T.);
#1899=FACE_OUTER_BOUND('',#2752,.T.);
#1900=FACE_OUTER_BOUND('',#2753,.T.);
#1901=FACE_OUTER_BOUND('',#2754,.T.);
#1902=FACE_OUTER_BOUND('',#2755,.T.);
#1903=FACE_OUTER_BOUND('',#2756,.T.);
#1904=FACE_OUTER_BOUND('',#2757,.T.);
#1905=FACE_OUTER_BOUND('',#2758,.T.);
#1906=FACE_OUTER_BOUND('',#2759,.T.);
#1907=FACE_OUTER_BOUND('',#2760,.T.);
#1908=FACE_OUTER_BOUND('',#2761,.T.);
#1909=FACE_OUTER_BOUND('',#2762,.T.);
#1910=FACE_OUTER_BOUND('',#2763,.T.);
#1911=FACE_OUTER_BOUND('',#2764,.T.);
#1912=FACE_OUTER_BOUND('',#2765,.T.);
#1913=FACE_OUTER_BOUND('',#2766,.T.);
#1914=FACE_OUTER_BOUND('',#2767,.T.);
#1915=FACE_OUTER_BOUND('',#2768,.T.);
#1916=FACE_OUTER_BOUND('',#2769,.T.);
#1917=FACE_OUTER_BOUND('',#2770,.T.);
#1918=FACE_OUTER_BOUND('',#2771,.T.);
#1919=FACE_OUTER_BOUND('',#2772,.T.);
#1920=FACE_OUTER_BOUND('',#2773,.T.);
#1921=FACE_OUTER_BOUND('',#2774,.T.);
#1922=FACE_OUTER_BOUND('',#2775,.T.);
#1923=FACE_OUTER_BOUND('',#2776,.T.);
#1924=FACE_OUTER_BOUND('',#2777,.T.);
#1925=FACE_OUTER_BOUND('',#2778,.T.);
#1926=FACE_OUTER_BOUND('',#2779,.T.);
#1927=FACE_OUTER_BOUND('',#2780,.T.);
#1928=FACE_OUTER_BOUND('',#2781,.T.);
#1929=FACE_OUTER_BOUND('',#2782,.T.);
#1930=FACE_OUTER_BOUND('',#2783,.T.);
#1931=FACE_OUTER_BOUND('',#2784,.T.);
#1932=FACE_OUTER_BOUND('',#2785,.T.);
#1933=FACE_OUTER_BOUND('',#2786,.T.);
#1934=FACE_OUTER_BOUND('',#2787,.T.);
#1935=FACE_OUTER_BOUND('',#2788,.T.);
#1936=FACE_OUTER_BOUND('',#2789,.T.);
#1937=FACE_OUTER_BOUND('',#2790,.T.);
#1938=FACE_OUTER_BOUND('',#2791,.T.);
#1939=FACE_OUTER_BOUND('',#2792,.T.);
#1940=FACE_OUTER_BOUND('',#2793,.T.);
#1941=FACE_OUTER_BOUND('',#2794,.T.);
#1942=FACE_OUTER_BOUND('',#2795,.T.);
#1943=FACE_OUTER_BOUND('',#2796,.T.);
#1944=FACE_OUTER_BOUND('',#2797,.T.);
#1945=FACE_OUTER_BOUND('',#2798,.T.);
#1946=FACE_OUTER_BOUND('',#2799,.T.);
#1947=FACE_OUTER_BOUND('',#2800,.T.);
#1948=FACE_OUTER_BOUND('',#2801,.T.);
#1949=FACE_OUTER_BOUND('',#2802,.T.);
#1950=FACE_OUTER_BOUND('',#2803,.T.);
#1951=FACE_OUTER_BOUND('',#2805,.T.);
#1952=FACE_OUTER_BOUND('',#2806,.T.);
#1953=FACE_OUTER_BOUND('',#2808,.T.);
#1954=FACE_OUTER_BOUND('',#2809,.T.);
#1955=FACE_OUTER_BOUND('',#2810,.T.);
#1956=FACE_OUTER_BOUND('',#2811,.T.);
#1957=FACE_OUTER_BOUND('',#2812,.T.);
#1958=FACE_OUTER_BOUND('',#2813,.T.);
#1959=FACE_OUTER_BOUND('',#2814,.T.);
#1960=FACE_OUTER_BOUND('',#2815,.T.);
#1961=FACE_OUTER_BOUND('',#2816,.T.);
#1962=FACE_OUTER_BOUND('',#2817,.T.);
#1963=FACE_OUTER_BOUND('',#2818,.T.);
#1964=FACE_OUTER_BOUND('',#2819,.T.);
#1965=FACE_OUTER_BOUND('',#2820,.T.);
#1966=FACE_OUTER_BOUND('',#2821,.T.);
#1967=FACE_OUTER_BOUND('',#2822,.T.);
#1968=FACE_OUTER_BOUND('',#2823,.T.);
#1969=FACE_OUTER_BOUND('',#2824,.T.);
#1970=FACE_OUTER_BOUND('',#2825,.T.);
#1971=FACE_OUTER_BOUND('',#2826,.T.);
#1972=FACE_OUTER_BOUND('',#2827,.T.);
#1973=FACE_OUTER_BOUND('',#2828,.T.);
#1974=FACE_OUTER_BOUND('',#2829,.T.);
#1975=FACE_OUTER_BOUND('',#2830,.T.);
#1976=FACE_OUTER_BOUND('',#2831,.T.);
#1977=FACE_OUTER_BOUND('',#2832,.T.);
#1978=FACE_OUTER_BOUND('',#2833,.T.);
#1979=FACE_OUTER_BOUND('',#2834,.T.);
#1980=FACE_OUTER_BOUND('',#2835,.T.);
#1981=FACE_OUTER_BOUND('',#2836,.T.);
#1982=FACE_OUTER_BOUND('',#2837,.T.);
#1983=FACE_OUTER_BOUND('',#2838,.T.);
#1984=FACE_OUTER_BOUND('',#2839,.T.);
#1985=FACE_OUTER_BOUND('',#2840,.T.);
#1986=FACE_OUTER_BOUND('',#2841,.T.);
#1987=FACE_OUTER_BOUND('',#2842,.T.);
#1988=FACE_OUTER_BOUND('',#2843,.T.);
#1989=FACE_OUTER_BOUND('',#2844,.T.);
#1990=FACE_OUTER_BOUND('',#2845,.T.);
#1991=FACE_OUTER_BOUND('',#2846,.T.);
#1992=FACE_OUTER_BOUND('',#2847,.T.);
#1993=FACE_OUTER_BOUND('',#2848,.T.);
#1994=FACE_OUTER_BOUND('',#2849,.T.);
#1995=FACE_OUTER_BOUND('',#2850,.T.);
#1996=FACE_OUTER_BOUND('',#2851,.T.);
#1997=FACE_OUTER_BOUND('',#2852,.T.);
#1998=FACE_OUTER_BOUND('',#2853,.T.);
#1999=FACE_OUTER_BOUND('',#2854,.T.);
#2000=FACE_OUTER_BOUND('',#2855,.T.);
#2001=FACE_OUTER_BOUND('',#2856,.T.);
#2002=FACE_OUTER_BOUND('',#2857,.T.);
#2003=FACE_OUTER_BOUND('',#2858,.T.);
#2004=FACE_OUTER_BOUND('',#2859,.T.);
#2005=FACE_OUTER_BOUND('',#2860,.T.);
#2006=FACE_OUTER_BOUND('',#2861,.T.);
#2007=FACE_OUTER_BOUND('',#2862,.T.);
#2008=FACE_OUTER_BOUND('',#2863,.T.);
#2009=FACE_OUTER_BOUND('',#2864,.T.);
#2010=FACE_OUTER_BOUND('',#2865,.T.);
#2011=FACE_OUTER_BOUND('',#2866,.T.);
#2012=FACE_OUTER_BOUND('',#2867,.T.);
#2013=FACE_OUTER_BOUND('',#2868,.T.);
#2014=FACE_OUTER_BOUND('',#2869,.T.);
#2015=FACE_OUTER_BOUND('',#2870,.T.);
#2016=FACE_OUTER_BOUND('',#2871,.T.);
#2017=FACE_OUTER_BOUND('',#2872,.T.);
#2018=FACE_OUTER_BOUND('',#2873,.T.);
#2019=FACE_OUTER_BOUND('',#2874,.T.);
#2020=FACE_OUTER_BOUND('',#2875,.T.);
#2021=FACE_OUTER_BOUND('',#2876,.T.);
#2022=FACE_OUTER_BOUND('',#2877,.T.);
#2023=FACE_OUTER_BOUND('',#2878,.T.);
#2024=FACE_OUTER_BOUND('',#2879,.T.);
#2025=FACE_OUTER_BOUND('',#2880,.T.);
#2026=FACE_OUTER_BOUND('',#2881,.T.);
#2027=FACE_OUTER_BOUND('',#2882,.T.);
#2028=FACE_OUTER_BOUND('',#2883,.T.);
#2029=FACE_OUTER_BOUND('',#2884,.T.);
#2030=FACE_OUTER_BOUND('',#2885,.T.);
#2031=FACE_OUTER_BOUND('',#2886,.T.);
#2032=FACE_OUTER_BOUND('',#2887,.T.);
#2033=FACE_OUTER_BOUND('',#2888,.T.);
#2034=FACE_OUTER_BOUND('',#2889,.T.);
#2035=FACE_OUTER_BOUND('',#2890,.T.);
#2036=FACE_OUTER_BOUND('',#2891,.T.);
#2037=FACE_OUTER_BOUND('',#2892,.T.);
#2038=FACE_OUTER_BOUND('',#2893,.T.);
#2039=FACE_OUTER_BOUND('',#2894,.T.);
#2040=FACE_OUTER_BOUND('',#2895,.T.);
#2041=EDGE_LOOP('',(#8679,#8680,#8681,#8682));
#2042=EDGE_LOOP('',(#8683,#8684,#8685,#8686));
#2043=EDGE_LOOP('',(#8687,#8688,#8689,#8690));
#2044=EDGE_LOOP('',(#8691,#8692,#8693,#8694));
#2045=EDGE_LOOP('',(#8695,#8696,#8697,#8698));
#2046=EDGE_LOOP('',(#8699,#8700,#8701,#8702));
#2047=EDGE_LOOP('',(#8703,#8704,#8705,#8706));
#2048=EDGE_LOOP('',(#8707,#8708,#8709,#8710));
#2049=EDGE_LOOP('',(#8711,#8712,#8713,#8714));
#2050=EDGE_LOOP('',(#8715,#8716,#8717,#8718));
#2051=EDGE_LOOP('',(#8719));
#2052=EDGE_LOOP('',(#8720,#8721,#8722,#8723));
#2053=EDGE_LOOP('',(#8724,#8725,#8726,#8727));
#2054=EDGE_LOOP('',(#8728,#8729,#8730,#8731,#8732,#8733,#8734,#8735));
#2055=EDGE_LOOP('',(#8736,#8737,#8738,#8739,#8740,#8741,#8742,#8743));
#2056=EDGE_LOOP('',(#8744,#8745,#8746,#8747));
#2057=EDGE_LOOP('',(#8748,#8749,#8750,#8751));
#2058=EDGE_LOOP('',(#8752,#8753,#8754,#8755));
#2059=EDGE_LOOP('',(#8756,#8757,#8758,#8759));
#2060=EDGE_LOOP('',(#8760,#8761,#8762,#8763));
#2061=EDGE_LOOP('',(#8764,#8765,#8766,#8767));
#2062=EDGE_LOOP('',(#8768,#8769,#8770,#8771));
#2063=EDGE_LOOP('',(#8772,#8773,#8774,#8775));
#2064=EDGE_LOOP('',(#8776,#8777,#8778,#8779));
#2065=EDGE_LOOP('',(#8780,#8781,#8782,#8783));
#2066=EDGE_LOOP('',(#8784,#8785,#8786,#8787));
#2067=EDGE_LOOP('',(#8788,#8789,#8790,#8791));
#2068=EDGE_LOOP('',(#8792,#8793,#8794,#8795));
#2069=EDGE_LOOP('',(#8796,#8797,#8798,#8799));
#2070=EDGE_LOOP('',(#8800,#8801,#8802,#8803));
#2071=EDGE_LOOP('',(#8804,#8805,#8806,#8807));
#2072=EDGE_LOOP('',(#8808,#8809,#8810,#8811));
#2073=EDGE_LOOP('',(#8812,#8813,#8814,#8815));
#2074=EDGE_LOOP('',(#8816,#8817,#8818,#8819));
#2075=EDGE_LOOP('',(#8820,#8821,#8822,#8823));
#2076=EDGE_LOOP('',(#8824,#8825,#8826,#8827));
#2077=EDGE_LOOP('',(#8828,#8829,#8830,#8831,#8832,#8833,#8834,#8835));
#2078=EDGE_LOOP('',(#8836,#8837,#8838,#8839,#8840,#8841,#8842,#8843));
#2079=EDGE_LOOP('',(#8844,#8845,#8846,#8847));
#2080=EDGE_LOOP('',(#8848,#8849,#8850,#8851));
#2081=EDGE_LOOP('',(#8852,#8853,#8854,#8855));
#2082=EDGE_LOOP('',(#8856,#8857,#8858,#8859));
#2083=EDGE_LOOP('',(#8860,#8861,#8862,#8863));
#2084=EDGE_LOOP('',(#8864,#8865,#8866,#8867));
#2085=EDGE_LOOP('',(#8868,#8869,#8870,#8871));
#2086=EDGE_LOOP('',(#8872,#8873,#8874,#8875));
#2087=EDGE_LOOP('',(#8876,#8877,#8878,#8879));
#2088=EDGE_LOOP('',(#8880,#8881,#8882,#8883));
#2089=EDGE_LOOP('',(#8884,#8885,#8886,#8887));
#2090=EDGE_LOOP('',(#8888,#8889,#8890,#8891));
#2091=EDGE_LOOP('',(#8892,#8893,#8894,#8895));
#2092=EDGE_LOOP('',(#8896,#8897,#8898,#8899));
#2093=EDGE_LOOP('',(#8900,#8901,#8902,#8903));
#2094=EDGE_LOOP('',(#8904,#8905,#8906,#8907));
#2095=EDGE_LOOP('',(#8908));
#2096=EDGE_LOOP('',(#8909,#8910,#8911,#8912));
#2097=EDGE_LOOP('',(#8913,#8914,#8915,#8916));
#2098=EDGE_LOOP('',(#8917,#8918,#8919,#8920));
#2099=EDGE_LOOP('',(#8921,#8922,#8923,#8924));
#2100=EDGE_LOOP('',(#8925,#8926,#8927,#8928));
#2101=EDGE_LOOP('',(#8929,#8930,#8931,#8932));
#2102=EDGE_LOOP('',(#8933,#8934,#8935,#8936));
#2103=EDGE_LOOP('',(#8937,#8938,#8939,#8940,#8941,#8942));
#2104=EDGE_LOOP('',(#8943,#8944,#8945,#8946,#8947,#8948,#8949,#8950));
#2105=EDGE_LOOP('',(#8951,#8952,#8953,#8954,#8955,#8956,#8957,#8958,#8959,
#8960,#8961,#8962,#8963,#8964,#8965,#8966));
#2106=EDGE_LOOP('',(#8967,#8968,#8969,#8970));
#2107=EDGE_LOOP('',(#8971,#8972,#8973,#8974));
#2108=EDGE_LOOP('',(#8975,#8976,#8977,#8978));
#2109=EDGE_LOOP('',(#8979,#8980,#8981,#8982));
#2110=EDGE_LOOP('',(#8983,#8984,#8985,#8986));
#2111=EDGE_LOOP('',(#8987,#8988,#8989,#8990));
#2112=EDGE_LOOP('',(#8991,#8992,#8993,#8994));
#2113=EDGE_LOOP('',(#8995,#8996,#8997,#8998,#8999,#9000,#9001,#9002,#9003,
#9004,#9005,#9006));
#2114=EDGE_LOOP('',(#9007,#9008,#9009,#9010));
#2115=EDGE_LOOP('',(#9011,#9012,#9013,#9014));
#2116=EDGE_LOOP('',(#9015,#9016,#9017,#9018));
#2117=EDGE_LOOP('',(#9019,#9020,#9021,#9022));
#2118=EDGE_LOOP('',(#9023,#9024,#9025,#9026));
#2119=EDGE_LOOP('',(#9027,#9028,#9029,#9030));
#2120=EDGE_LOOP('',(#9031,#9032,#9033,#9034));
#2121=EDGE_LOOP('',(#9035,#9036,#9037,#9038,#9039,#9040));
#2122=EDGE_LOOP('',(#9041,#9042,#9043,#9044,#9045,#9046,#9047,#9048,#9049,
#9050,#9051,#9052,#9053,#9054,#9055,#9056));
#2123=EDGE_LOOP('',(#9057,#9058,#9059,#9060));
#2124=EDGE_LOOP('',(#9061,#9062,#9063,#9064));
#2125=EDGE_LOOP('',(#9065,#9066,#9067,#9068));
#2126=EDGE_LOOP('',(#9069,#9070,#9071,#9072));
#2127=EDGE_LOOP('',(#9073,#9074,#9075,#9076));
#2128=EDGE_LOOP('',(#9077,#9078,#9079,#9080));
#2129=EDGE_LOOP('',(#9081,#9082,#9083,#9084));
#2130=EDGE_LOOP('',(#9085,#9086,#9087,#9088,#9089,#9090,#9091,#9092,#9093,
#9094,#9095,#9096));
#2131=EDGE_LOOP('',(#9097,#9098,#9099,#9100,#9101));
#2132=EDGE_LOOP('',(#9102,#9103,#9104,#9105,#9106,#9107,#9108,#9109));
#2133=EDGE_LOOP('',(#9110,#9111,#9112,#9113,#9114,#9115));
#2134=EDGE_LOOP('',(#9116,#9117,#9118,#9119,#9120));
#2135=EDGE_LOOP('',(#9121,#9122,#9123,#9124));
#2136=EDGE_LOOP('',(#9125,#9126,#9127,#9128,#9129,#9130,#9131,#9132));
#2137=EDGE_LOOP('',(#9133,#9134,#9135,#9136));
#2138=EDGE_LOOP('',(#9137,#9138,#9139,#9140));
#2139=EDGE_LOOP('',(#9141,#9142,#9143,#9144,#9145));
#2140=EDGE_LOOP('',(#9146,#9147,#9148,#9149,#9150,#9151));
#2141=EDGE_LOOP('',(#9152,#9153,#9154,#9155,#9156));
#2142=EDGE_LOOP('',(#9157,#9158,#9159,#9160));
#2143=EDGE_LOOP('',(#9161,#9162,#9163,#9164));
#2144=EDGE_LOOP('',(#9165,#9166,#9167,#9168));
#2145=EDGE_LOOP('',(#9169,#9170,#9171,#9172));
#2146=EDGE_LOOP('',(#9173,#9174,#9175,#9176));
#2147=EDGE_LOOP('',(#9177,#9178,#9179,#9180,#9181,#9182));
#2148=EDGE_LOOP('',(#9183,#9184,#9185,#9186));
#2149=EDGE_LOOP('',(#9187,#9188,#9189,#9190,#9191,#9192));
#2150=EDGE_LOOP('',(#9193,#9194,#9195,#9196,#9197,#9198,#9199,#9200));
#2151=EDGE_LOOP('',(#9201,#9202,#9203,#9204));
#2152=EDGE_LOOP('',(#9205,#9206,#9207,#9208));
#2153=EDGE_LOOP('',(#9209,#9210,#9211,#9212));
#2154=EDGE_LOOP('',(#9213,#9214,#9215,#9216));
#2155=EDGE_LOOP('',(#9217,#9218,#9219,#9220));
#2156=EDGE_LOOP('',(#9221,#9222,#9223,#9224,#9225,#9226));
#2157=EDGE_LOOP('',(#9227,#9228,#9229,#9230));
#2158=EDGE_LOOP('',(#9231,#9232,#9233,#9234,#9235,#9236));
#2159=EDGE_LOOP('',(#9237,#9238,#9239,#9240));
#2160=EDGE_LOOP('',(#9241,#9242,#9243,#9244));
#2161=EDGE_LOOP('',(#9245,#9246,#9247,#9248));
#2162=EDGE_LOOP('',(#9249,#9250,#9251,#9252));
#2163=EDGE_LOOP('',(#9253,#9254,#9255,#9256));
#2164=EDGE_LOOP('',(#9257,#9258,#9259,#9260));
#2165=EDGE_LOOP('',(#9261,#9262,#9263,#9264));
#2166=EDGE_LOOP('',(#9265,#9266,#9267,#9268));
#2167=EDGE_LOOP('',(#9269,#9270,#9271,#9272));
#2168=EDGE_LOOP('',(#9273,#9274,#9275,#9276));
#2169=EDGE_LOOP('',(#9277,#9278,#9279,#9280,#9281,#9282));
#2170=EDGE_LOOP('',(#9283,#9284,#9285,#9286));
#2171=EDGE_LOOP('',(#9287,#9288,#9289,#9290,#9291,#9292));
#2172=EDGE_LOOP('',(#9293,#9294,#9295,#9296,#9297,#9298));
#2173=EDGE_LOOP('',(#9299,#9300,#9301,#9302,#9303,#9304,#9305,#9306));
#2174=EDGE_LOOP('',(#9307,#9308,#9309,#9310,#9311,#9312));
#2175=EDGE_LOOP('',(#9313,#9314,#9315,#9316));
#2176=EDGE_LOOP('',(#9317,#9318,#9319,#9320));
#2177=EDGE_LOOP('',(#9321,#9322,#9323,#9324));
#2178=EDGE_LOOP('',(#9325,#9326,#9327,#9328));
#2179=EDGE_LOOP('',(#9329));
#2180=EDGE_LOOP('',(#9330,#9331,#9332,#9333));
#2181=EDGE_LOOP('',(#9334,#9335,#9336,#9337));
#2182=EDGE_LOOP('',(#9338));
#2183=EDGE_LOOP('',(#9339,#9340,#9341,#9342));
#2184=EDGE_LOOP('',(#9343,#9344,#9345,#9346));
#2185=EDGE_LOOP('',(#9347,#9348,#9349,#9350));
#2186=EDGE_LOOP('',(#9351,#9352,#9353,#9354));
#2187=EDGE_LOOP('',(#9355,#9356,#9357,#9358));
#2188=EDGE_LOOP('',(#9359,#9360,#9361,#9362));
#2189=EDGE_LOOP('',(#9363,#9364,#9365,#9366));
#2190=EDGE_LOOP('',(#9367,#9368,#9369,#9370));
#2191=EDGE_LOOP('',(#9371,#9372,#9373,#9374));
#2192=EDGE_LOOP('',(#9375,#9376,#9377,#9378));
#2193=EDGE_LOOP('',(#9379,#9380,#9381,#9382));
#2194=EDGE_LOOP('',(#9383,#9384,#9385,#9386));
#2195=EDGE_LOOP('',(#9387,#9388,#9389,#9390,#9391,#9392,#9393,#9394));
#2196=EDGE_LOOP('',(#9395,#9396,#9397,#9398,#9399,#9400,#9401,#9402));
#2197=EDGE_LOOP('',(#9403,#9404,#9405,#9406));
#2198=EDGE_LOOP('',(#9407,#9408,#9409,#9410));
#2199=EDGE_LOOP('',(#9411,#9412,#9413,#9414));
#2200=EDGE_LOOP('',(#9415,#9416,#9417,#9418));
#2201=EDGE_LOOP('',(#9419,#9420,#9421,#9422));
#2202=EDGE_LOOP('',(#9423,#9424,#9425,#9426));
#2203=EDGE_LOOP('',(#9427,#9428,#9429,#9430));
#2204=EDGE_LOOP('',(#9431,#9432,#9433,#9434));
#2205=EDGE_LOOP('',(#9435,#9436,#9437,#9438));
#2206=EDGE_LOOP('',(#9439,#9440,#9441,#9442));
#2207=EDGE_LOOP('',(#9443,#9444,#9445,#9446));
#2208=EDGE_LOOP('',(#9447,#9448,#9449,#9450));
#2209=EDGE_LOOP('',(#9451,#9452,#9453,#9454));
#2210=EDGE_LOOP('',(#9455,#9456,#9457,#9458));
#2211=EDGE_LOOP('',(#9459,#9460,#9461,#9462));
#2212=EDGE_LOOP('',(#9463,#9464,#9465,#9466));
#2213=EDGE_LOOP('',(#9467,#9468,#9469,#9470));
#2214=EDGE_LOOP('',(#9471,#9472,#9473,#9474));
#2215=EDGE_LOOP('',(#9475,#9476,#9477,#9478));
#2216=EDGE_LOOP('',(#9479,#9480,#9481,#9482));
#2217=EDGE_LOOP('',(#9483,#9484,#9485,#9486,#9487,#9488,#9489,#9490));
#2218=EDGE_LOOP('',(#9491,#9492,#9493,#9494,#9495,#9496,#9497,#9498));
#2219=EDGE_LOOP('',(#9499,#9500,#9501,#9502));
#2220=EDGE_LOOP('',(#9503,#9504,#9505,#9506));
#2221=EDGE_LOOP('',(#9507,#9508,#9509,#9510));
#2222=EDGE_LOOP('',(#9511,#9512,#9513,#9514));
#2223=EDGE_LOOP('',(#9515,#9516,#9517,#9518));
#2224=EDGE_LOOP('',(#9519,#9520,#9521,#9522));
#2225=EDGE_LOOP('',(#9523,#9524,#9525,#9526));
#2226=EDGE_LOOP('',(#9527,#9528,#9529,#9530));
#2227=EDGE_LOOP('',(#9531,#9532,#9533,#9534));
#2228=EDGE_LOOP('',(#9535,#9536,#9537,#9538));
#2229=EDGE_LOOP('',(#9539,#9540,#9541,#9542));
#2230=EDGE_LOOP('',(#9543,#9544,#9545,#9546));
#2231=EDGE_LOOP('',(#9547,#9548,#9549,#9550));
#2232=EDGE_LOOP('',(#9551,#9552,#9553,#9554));
#2233=EDGE_LOOP('',(#9555,#9556,#9557,#9558));
#2234=EDGE_LOOP('',(#9559,#9560,#9561,#9562));
#2235=EDGE_LOOP('',(#9563));
#2236=EDGE_LOOP('',(#9564));
#2237=EDGE_LOOP('',(#9565));
#2238=EDGE_LOOP('',(#9566));
#2239=EDGE_LOOP('',(#9567));
#2240=EDGE_LOOP('',(#9568));
#2241=EDGE_LOOP('',(#9569,#9570,#9571,#9572));
#2242=EDGE_LOOP('',(#9573,#9574,#9575,#9576));
#2243=EDGE_LOOP('',(#9577,#9578,#9579,#9580));
#2244=EDGE_LOOP('',(#9581,#9582,#9583,#9584));
#2245=EDGE_LOOP('',(#9585,#9586,#9587,#9588));
#2246=EDGE_LOOP('',(#9589,#9590,#9591,#9592));
#2247=EDGE_LOOP('',(#9593,#9594,#9595,#9596));
#2248=EDGE_LOOP('',(#9597,#9598,#9599,#9600));
#2249=EDGE_LOOP('',(#9601,#9602,#9603,#9604));
#2250=EDGE_LOOP('',(#9605,#9606,#9607,#9608));
#2251=EDGE_LOOP('',(#9609,#9610,#9611,#9612));
#2252=EDGE_LOOP('',(#9613,#9614,#9615,#9616));
#2253=EDGE_LOOP('',(#9617,#9618,#9619,#9620));
#2254=EDGE_LOOP('',(#9621));
#2255=EDGE_LOOP('',(#9622));
#2256=EDGE_LOOP('',(#9623));
#2257=EDGE_LOOP('',(#9624));
#2258=EDGE_LOOP('',(#9625));
#2259=EDGE_LOOP('',(#9626));
#2260=EDGE_LOOP('',(#9627));
#2261=EDGE_LOOP('',(#9628,#9629,#9630,#9631));
#2262=EDGE_LOOP('',(#9632,#9633,#9634,#9635));
#2263=EDGE_LOOP('',(#9636,#9637,#9638,#9639));
#2264=EDGE_LOOP('',(#9640,#9641,#9642,#9643));
#2265=EDGE_LOOP('',(#9644,#9645,#9646,#9647));
#2266=EDGE_LOOP('',(#9648,#9649,#9650,#9651));
#2267=EDGE_LOOP('',(#9652,#9653,#9654,#9655));
#2268=EDGE_LOOP('',(#9656,#9657,#9658,#9659));
#2269=EDGE_LOOP('',(#9660,#9661,#9662,#9663));
#2270=EDGE_LOOP('',(#9664,#9665,#9666,#9667));
#2271=EDGE_LOOP('',(#9668,#9669,#9670,#9671));
#2272=EDGE_LOOP('',(#9672,#9673,#9674,#9675,#9676,#9677,#9678,#9679));
#2273=EDGE_LOOP('',(#9680,#9681,#9682,#9683,#9684,#9685,#9686,#9687));
#2274=EDGE_LOOP('',(#9688,#9689,#9690,#9691));
#2275=EDGE_LOOP('',(#9692,#9693,#9694,#9695));
#2276=EDGE_LOOP('',(#9696,#9697,#9698,#9699));
#2277=EDGE_LOOP('',(#9700,#9701,#9702,#9703));
#2278=EDGE_LOOP('',(#9704,#9705,#9706,#9707));
#2279=EDGE_LOOP('',(#9708,#9709,#9710,#9711));
#2280=EDGE_LOOP('',(#9712,#9713,#9714,#9715));
#2281=EDGE_LOOP('',(#9716,#9717,#9718,#9719));
#2282=EDGE_LOOP('',(#9720,#9721,#9722,#9723));
#2283=EDGE_LOOP('',(#9724,#9725,#9726,#9727));
#2284=EDGE_LOOP('',(#9728,#9729,#9730,#9731));
#2285=EDGE_LOOP('',(#9732,#9733,#9734,#9735));
#2286=EDGE_LOOP('',(#9736,#9737,#9738,#9739));
#2287=EDGE_LOOP('',(#9740,#9741,#9742,#9743));
#2288=EDGE_LOOP('',(#9744));
#2289=EDGE_LOOP('',(#9745));
#2290=EDGE_LOOP('',(#9746));
#2291=EDGE_LOOP('',(#9747));
#2292=EDGE_LOOP('',(#9748));
#2293=EDGE_LOOP('',(#9749));
#2294=EDGE_LOOP('',(#9750));
#2295=EDGE_LOOP('',(#9751,#9752,#9753,#9754));
#2296=EDGE_LOOP('',(#9755,#9756,#9757,#9758));
#2297=EDGE_LOOP('',(#9759,#9760,#9761,#9762));
#2298=EDGE_LOOP('',(#9763,#9764,#9765,#9766));
#2299=EDGE_LOOP('',(#9767,#9768,#9769,#9770));
#2300=EDGE_LOOP('',(#9771,#9772,#9773,#9774));
#2301=EDGE_LOOP('',(#9775,#9776,#9777,#9778));
#2302=EDGE_LOOP('',(#9779,#9780,#9781,#9782));
#2303=EDGE_LOOP('',(#9783,#9784,#9785,#9786));
#2304=EDGE_LOOP('',(#9787,#9788,#9789,#9790));
#2305=EDGE_LOOP('',(#9791,#9792,#9793,#9794));
#2306=EDGE_LOOP('',(#9795,#9796,#9797,#9798));
#2307=EDGE_LOOP('',(#9799,#9800,#9801,#9802));
#2308=EDGE_LOOP('',(#9803,#9804,#9805,#9806));
#2309=EDGE_LOOP('',(#9807,#9808,#9809,#9810));
#2310=EDGE_LOOP('',(#9811,#9812,#9813,#9814));
#2311=EDGE_LOOP('',(#9815,#9816,#9817,#9818));
#2312=EDGE_LOOP('',(#9819));
#2313=EDGE_LOOP('',(#9820));
#2314=EDGE_LOOP('',(#9821));
#2315=EDGE_LOOP('',(#9822));
#2316=EDGE_LOOP('',(#9823));
#2317=EDGE_LOOP('',(#9824));
#2318=EDGE_LOOP('',(#9825,#9826,#9827,#9828));
#2319=EDGE_LOOP('',(#9829,#9830,#9831,#9832));
#2320=EDGE_LOOP('',(#9833,#9834,#9835,#9836));
#2321=EDGE_LOOP('',(#9837,#9838,#9839,#9840));
#2322=EDGE_LOOP('',(#9841,#9842,#9843,#9844));
#2323=EDGE_LOOP('',(#9845,#9846,#9847,#9848));
#2324=EDGE_LOOP('',(#9849,#9850,#9851,#9852));
#2325=EDGE_LOOP('',(#9853,#9854,#9855,#9856));
#2326=EDGE_LOOP('',(#9857,#9858,#9859,#9860));
#2327=EDGE_LOOP('',(#9861,#9862,#9863,#9864));
#2328=EDGE_LOOP('',(#9865,#9866,#9867,#9868));
#2329=EDGE_LOOP('',(#9869,#9870,#9871,#9872));
#2330=EDGE_LOOP('',(#9873,#9874,#9875,#9876));
#2331=EDGE_LOOP('',(#9877,#9878,#9879,#9880));
#2332=EDGE_LOOP('',(#9881,#9882,#9883,#9884));
#2333=EDGE_LOOP('',(#9885,#9886,#9887,#9888,#9889,#9890,#9891,#9892));
#2334=EDGE_LOOP('',(#9893,#9894,#9895,#9896,#9897,#9898,#9899,#9900));
#2335=EDGE_LOOP('',(#9901,#9902,#9903,#9904));
#2336=EDGE_LOOP('',(#9905,#9906,#9907,#9908));
#2337=EDGE_LOOP('',(#9909,#9910,#9911,#9912));
#2338=EDGE_LOOP('',(#9913,#9914,#9915,#9916));
#2339=EDGE_LOOP('',(#9917,#9918,#9919,#9920));
#2340=EDGE_LOOP('',(#9921,#9922,#9923,#9924));
#2341=EDGE_LOOP('',(#9925,#9926,#9927,#9928));
#2342=EDGE_LOOP('',(#9929,#9930,#9931,#9932));
#2343=EDGE_LOOP('',(#9933,#9934,#9935,#9936));
#2344=EDGE_LOOP('',(#9937,#9938,#9939,#9940));
#2345=EDGE_LOOP('',(#9941,#9942,#9943,#9944));
#2346=EDGE_LOOP('',(#9945,#9946,#9947,#9948));
#2347=EDGE_LOOP('',(#9949,#9950,#9951,#9952));
#2348=EDGE_LOOP('',(#9953,#9954,#9955,#9956));
#2349=EDGE_LOOP('',(#9957,#9958,#9959,#9960));
#2350=EDGE_LOOP('',(#9961,#9962,#9963,#9964));
#2351=EDGE_LOOP('',(#9965,#9966,#9967,#9968));
#2352=EDGE_LOOP('',(#9969,#9970,#9971,#9972));
#2353=EDGE_LOOP('',(#9973,#9974,#9975,#9976));
#2354=EDGE_LOOP('',(#9977,#9978,#9979,#9980));
#2355=EDGE_LOOP('',(#9981,#9982,#9983,#9984));
#2356=EDGE_LOOP('',(#9985,#9986,#9987,#9988));
#2357=EDGE_LOOP('',(#9989,#9990,#9991,#9992,#9993));
#2358=EDGE_LOOP('',(#9994,#9995,#9996,#9997,#9998,#9999));
#2359=EDGE_LOOP('',(#10000,#10001,#10002,#10003,#10004,#10005,#10006,#10007,
#10008,#10009,#10010,#10011,#10012,#10013,#10014,#10015));
#2360=EDGE_LOOP('',(#10016,#10017,#10018,#10019));
#2361=EDGE_LOOP('',(#10020,#10021,#10022,#10023));
#2362=EDGE_LOOP('',(#10024,#10025,#10026,#10027));
#2363=EDGE_LOOP('',(#10028,#10029,#10030,#10031));
#2364=EDGE_LOOP('',(#10032,#10033,#10034,#10035));
#2365=EDGE_LOOP('',(#10036,#10037,#10038,#10039));
#2366=EDGE_LOOP('',(#10040,#10041,#10042,#10043));
#2367=EDGE_LOOP('',(#10044,#10045,#10046,#10047,#10048,#10049));
#2368=EDGE_LOOP('',(#10050,#10051,#10052,#10053,#10054));
#2369=EDGE_LOOP('',(#10055,#10056,#10057,#10058,#10059,#10060,#10061,#10062,
#10063,#10064,#10065,#10066));
#2370=EDGE_LOOP('',(#10067,#10068,#10069,#10070));
#2371=EDGE_LOOP('',(#10071,#10072,#10073,#10074));
#2372=EDGE_LOOP('',(#10075,#10076,#10077,#10078));
#2373=EDGE_LOOP('',(#10079,#10080,#10081,#10082));
#2374=EDGE_LOOP('',(#10083,#10084,#10085,#10086));
#2375=EDGE_LOOP('',(#10087,#10088,#10089,#10090));
#2376=EDGE_LOOP('',(#10091,#10092,#10093,#10094));
#2377=EDGE_LOOP('',(#10095,#10096,#10097,#10098,#10099,#10100));
#2378=EDGE_LOOP('',(#10101,#10102,#10103,#10104,#10105,#10106,#10107,#10108));
#2379=EDGE_LOOP('',(#10109,#10110,#10111,#10112));
#2380=EDGE_LOOP('',(#10113,#10114,#10115,#10116));
#2381=EDGE_LOOP('',(#10117,#10118,#10119,#10120));
#2382=EDGE_LOOP('',(#10121,#10122,#10123,#10124));
#2383=EDGE_LOOP('',(#10125,#10126,#10127,#10128));
#2384=EDGE_LOOP('',(#10129,#10130,#10131,#10132));
#2385=EDGE_LOOP('',(#10133,#10134,#10135,#10136));
#2386=EDGE_LOOP('',(#10137,#10138,#10139,#10140,#10141,#10142,#10143,#10144,
#10145,#10146,#10147,#10148));
#2387=EDGE_LOOP('',(#10149,#10150,#10151,#10152,#10153,#10154,#10155,#10156,
#10157,#10158,#10159,#10160,#10161,#10162,#10163,#10164));
#2388=EDGE_LOOP('',(#10165,#10166,#10167,#10168,#10169,#10170));
#2389=EDGE_LOOP('',(#10171,#10172,#10173,#10174,#10175));
#2390=EDGE_LOOP('',(#10176,#10177,#10178,#10179,#10180,#10181,#10182,#10183));
#2391=EDGE_LOOP('',(#10184,#10185,#10186,#10187));
#2392=EDGE_LOOP('',(#10188,#10189,#10190,#10191,#10192,#10193,#10194,#10195));
#2393=EDGE_LOOP('',(#10196,#10197,#10198,#10199));
#2394=EDGE_LOOP('',(#10200,#10201,#10202,#10203));
#2395=EDGE_LOOP('',(#10204,#10205,#10206,#10207,#10208));
#2396=EDGE_LOOP('',(#10209,#10210,#10211,#10212));
#2397=EDGE_LOOP('',(#10213,#10214,#10215,#10216));
#2398=EDGE_LOOP('',(#10217,#10218,#10219,#10220));
#2399=EDGE_LOOP('',(#10221,#10222,#10223,#10224));
#2400=EDGE_LOOP('',(#10225,#10226,#10227,#10228));
#2401=EDGE_LOOP('',(#10229,#10230,#10231,#10232,#10233,#10234,#10235,#10236));
#2402=EDGE_LOOP('',(#10237,#10238,#10239,#10240,#10241,#10242));
#2403=EDGE_LOOP('',(#10243,#10244,#10245,#10246));
#2404=EDGE_LOOP('',(#10247,#10248,#10249,#10250,#10251,#10252));
#2405=EDGE_LOOP('',(#10253,#10254,#10255,#10256));
#2406=EDGE_LOOP('',(#10257,#10258,#10259,#10260));
#2407=EDGE_LOOP('',(#10261,#10262,#10263,#10264));
#2408=EDGE_LOOP('',(#10265,#10266,#10267,#10268));
#2409=EDGE_LOOP('',(#10269,#10270,#10271,#10272));
#2410=EDGE_LOOP('',(#10273,#10274,#10275,#10276));
#2411=EDGE_LOOP('',(#10277,#10278,#10279,#10280));
#2412=EDGE_LOOP('',(#10281,#10282,#10283,#10284));
#2413=EDGE_LOOP('',(#10285,#10286,#10287,#10288));
#2414=EDGE_LOOP('',(#10289,#10290,#10291,#10292));
#2415=EDGE_LOOP('',(#10293,#10294,#10295,#10296,#10297,#10298));
#2416=EDGE_LOOP('',(#10299,#10300,#10301,#10302));
#2417=EDGE_LOOP('',(#10303,#10304,#10305,#10306,#10307,#10308));
#2418=EDGE_LOOP('',(#10309,#10310,#10311,#10312,#10313,#10314,#10315,#10316));
#2419=EDGE_LOOP('',(#10317,#10318,#10319,#10320));
#2420=EDGE_LOOP('',(#10321,#10322,#10323,#10324));
#2421=EDGE_LOOP('',(#10325,#10326,#10327,#10328));
#2422=EDGE_LOOP('',(#10329,#10330,#10331,#10332));
#2423=EDGE_LOOP('',(#10333,#10334,#10335,#10336));
#2424=EDGE_LOOP('',(#10337,#10338,#10339,#10340,#10341,#10342));
#2425=EDGE_LOOP('',(#10343,#10344,#10345,#10346));
#2426=EDGE_LOOP('',(#10347,#10348,#10349,#10350,#10351,#10352));
#2427=EDGE_LOOP('',(#10353,#10354,#10355,#10356,#10357,#10358));
#2428=EDGE_LOOP('',(#10359,#10360,#10361,#10362));
#2429=EDGE_LOOP('',(#10363,#10364,#10365,#10366,#10367,#10368));
#2430=EDGE_LOOP('',(#10369,#10370,#10371,#10372));
#2431=EDGE_LOOP('',(#10373,#10374,#10375,#10376));
#2432=EDGE_LOOP('',(#10377,#10378,#10379,#10380));
#2433=EDGE_LOOP('',(#10381,#10382,#10383,#10384,#10385,#10386,#10387));
#2434=EDGE_LOOP('',(#10388,#10389,#10390,#10391));
#2435=EDGE_LOOP('',(#10392));
#2436=EDGE_LOOP('',(#10393,#10394,#10395,#10396,#10397,#10398,#10399));
#2437=EDGE_LOOP('',(#10400,#10401,#10402,#10403));
#2438=EDGE_LOOP('',(#10404,#10405,#10406,#10407,#10408,#10409,#10410,#10411));
#2439=EDGE_LOOP('',(#10412));
#2440=EDGE_LOOP('',(#10413,#10414,#10415,#10416));
#2441=EDGE_LOOP('',(#10417,#10418,#10419,#10420));
#2442=EDGE_LOOP('',(#10421,#10422,#10423,#10424));
#2443=EDGE_LOOP('',(#10425,#10426,#10427,#10428));
#2444=EDGE_LOOP('',(#10429,#10430,#10431,#10432,#10433,#10434,#10435));
#2445=EDGE_LOOP('',(#10436,#10437,#10438,#10439));
#2446=EDGE_LOOP('',(#10440));
#2447=EDGE_LOOP('',(#10441,#10442,#10443,#10444,#10445,#10446,#10447));
#2448=EDGE_LOOP('',(#10448,#10449,#10450,#10451));
#2449=EDGE_LOOP('',(#10452,#10453,#10454,#10455));
#2450=EDGE_LOOP('',(#10456,#10457,#10458,#10459));
#2451=EDGE_LOOP('',(#10460,#10461,#10462,#10463));
#2452=EDGE_LOOP('',(#10464,#10465,#10466,#10467));
#2453=EDGE_LOOP('',(#10468,#10469,#10470,#10471,#10472,#10473,#10474,#10475,
#10476,#10477,#10478,#10479,#10480,#10481));
#2454=EDGE_LOOP('',(#10482,#10483,#10484,#10485));
#2455=EDGE_LOOP('',(#10486,#10487,#10488,#10489));
#2456=EDGE_LOOP('',(#10490,#10491,#10492,#10493));
#2457=EDGE_LOOP('',(#10494,#10495,#10496,#10497,#10498,#10499,#10500,#10501,
#10502,#10503,#10504,#10505,#10506,#10507));
#2458=EDGE_LOOP('',(#10508,#10509,#10510,#10511));
#2459=EDGE_LOOP('',(#10512,#10513,#10514,#10515));
#2460=EDGE_LOOP('',(#10516,#10517,#10518,#10519));
#2461=EDGE_LOOP('',(#10520,#10521,#10522,#10523));
#2462=EDGE_LOOP('',(#10524,#10525,#10526,#10527));
#2463=EDGE_LOOP('',(#10528,#10529,#10530,#10531));
#2464=EDGE_LOOP('',(#10532,#10533,#10534,#10535));
#2465=EDGE_LOOP('',(#10536,#10537,#10538,#10539));
#2466=EDGE_LOOP('',(#10540,#10541,#10542,#10543));
#2467=EDGE_LOOP('',(#10544,#10545,#10546,#10547));
#2468=EDGE_LOOP('',(#10548,#10549,#10550,#10551));
#2469=EDGE_LOOP('',(#10552,#10553,#10554,#10555));
#2470=EDGE_LOOP('',(#10556,#10557,#10558,#10559));
#2471=EDGE_LOOP('',(#10560,#10561,#10562,#10563));
#2472=EDGE_LOOP('',(#10564,#10565,#10566,#10567));
#2473=EDGE_LOOP('',(#10568,#10569,#10570,#10571));
#2474=EDGE_LOOP('',(#10572,#10573,#10574,#10575));
#2475=EDGE_LOOP('',(#10576,#10577,#10578,#10579));
#2476=EDGE_LOOP('',(#10580,#10581,#10582,#10583));
#2477=EDGE_LOOP('',(#10584,#10585,#10586,#10587));
#2478=EDGE_LOOP('',(#10588,#10589,#10590,#10591));
#2479=EDGE_LOOP('',(#10592,#10593,#10594,#10595));
#2480=EDGE_LOOP('',(#10596,#10597,#10598,#10599));
#2481=EDGE_LOOP('',(#10600,#10601,#10602,#10603));
#2482=EDGE_LOOP('',(#10604,#10605,#10606,#10607));
#2483=EDGE_LOOP('',(#10608,#10609,#10610,#10611));
#2484=EDGE_LOOP('',(#10612,#10613,#10614,#10615));
#2485=EDGE_LOOP('',(#10616,#10617,#10618,#10619));
#2486=EDGE_LOOP('',(#10620,#10621,#10622,#10623));
#2487=EDGE_LOOP('',(#10624,#10625,#10626,#10627,#10628,#10629,#10630,#10631));
#2488=EDGE_LOOP('',(#10632,#10633,#10634,#10635));
#2489=EDGE_LOOP('',(#10636,#10637,#10638,#10639));
#2490=EDGE_LOOP('',(#10640,#10641,#10642,#10643));
#2491=EDGE_LOOP('',(#10644,#10645,#10646,#10647));
#2492=EDGE_LOOP('',(#10648,#10649,#10650,#10651));
#2493=EDGE_LOOP('',(#10652,#10653,#10654,#10655));
#2494=EDGE_LOOP('',(#10656,#10657,#10658,#10659));
#2495=EDGE_LOOP('',(#10660,#10661,#10662,#10663));
#2496=EDGE_LOOP('',(#10664,#10665,#10666,#10667));
#2497=EDGE_LOOP('',(#10668,#10669,#10670,#10671,#10672,#10673));
#2498=EDGE_LOOP('',(#10674,#10675,#10676,#10677));
#2499=EDGE_LOOP('',(#10678,#10679,#10680,#10681));
#2500=EDGE_LOOP('',(#10682,#10683,#10684,#10685));
#2501=EDGE_LOOP('',(#10686,#10687,#10688,#10689));
#2502=EDGE_LOOP('',(#10690,#10691,#10692,#10693));
#2503=EDGE_LOOP('',(#10694,#10695,#10696,#10697,#10698,#10699));
#2504=EDGE_LOOP('',(#10700,#10701,#10702,#10703));
#2505=EDGE_LOOP('',(#10704,#10705,#10706,#10707));
#2506=EDGE_LOOP('',(#10708,#10709,#10710,#10711));
#2507=EDGE_LOOP('',(#10712,#10713,#10714,#10715));
#2508=EDGE_LOOP('',(#10716,#10717,#10718,#10719));
#2509=EDGE_LOOP('',(#10720,#10721,#10722,#10723));
#2510=EDGE_LOOP('',(#10724));
#2511=EDGE_LOOP('',(#10725,#10726,#10727,#10728));
#2512=EDGE_LOOP('',(#10729,#10730,#10731,#10732));
#2513=EDGE_LOOP('',(#10733,#10734,#10735,#10736));
#2514=EDGE_LOOP('',(#10737,#10738,#10739,#10740));
#2515=EDGE_LOOP('',(#10741,#10742,#10743,#10744));
#2516=EDGE_LOOP('',(#10745,#10746,#10747,#10748));
#2517=EDGE_LOOP('',(#10749));
#2518=EDGE_LOOP('',(#10750,#10751,#10752,#10753));
#2519=EDGE_LOOP('',(#10754,#10755,#10756,#10757));
#2520=EDGE_LOOP('',(#10758,#10759,#10760,#10761));
#2521=EDGE_LOOP('',(#10762,#10763,#10764,#10765));
#2522=EDGE_LOOP('',(#10766,#10767,#10768,#10769));
#2523=EDGE_LOOP('',(#10770,#10771,#10772,#10773));
#2524=EDGE_LOOP('',(#10774));
#2525=EDGE_LOOP('',(#10775,#10776,#10777,#10778));
#2526=EDGE_LOOP('',(#10779,#10780,#10781,#10782));
#2527=EDGE_LOOP('',(#10783,#10784,#10785,#10786));
#2528=EDGE_LOOP('',(#10787,#10788,#10789,#10790));
#2529=EDGE_LOOP('',(#10791,#10792,#10793,#10794));
#2530=EDGE_LOOP('',(#10795,#10796,#10797,#10798));
#2531=EDGE_LOOP('',(#10799));
#2532=EDGE_LOOP('',(#10800,#10801,#10802,#10803));
#2533=EDGE_LOOP('',(#10804,#10805,#10806,#10807));
#2534=EDGE_LOOP('',(#10808,#10809,#10810,#10811));
#2535=EDGE_LOOP('',(#10812,#10813,#10814,#10815));
#2536=EDGE_LOOP('',(#10816,#10817,#10818,#10819));
#2537=EDGE_LOOP('',(#10820,#10821,#10822,#10823));
#2538=EDGE_LOOP('',(#10824,#10825,#10826,#10827));
#2539=EDGE_LOOP('',(#10828));
#2540=EDGE_LOOP('',(#10829,#10830,#10831,#10832));
#2541=EDGE_LOOP('',(#10833,#10834,#10835,#10836));
#2542=EDGE_LOOP('',(#10837,#10838,#10839,#10840));
#2543=EDGE_LOOP('',(#10841));
#2544=EDGE_LOOP('',(#10842,#10843,#10844,#10845));
#2545=EDGE_LOOP('',(#10846,#10847,#10848,#10849));
#2546=EDGE_LOOP('',(#10850,#10851,#10852,#10853));
#2547=EDGE_LOOP('',(#10854));
#2548=EDGE_LOOP('',(#10855,#10856,#10857,#10858));
#2549=EDGE_LOOP('',(#10859,#10860,#10861,#10862));
#2550=EDGE_LOOP('',(#10863,#10864,#10865,#10866));
#2551=EDGE_LOOP('',(#10867));
#2552=EDGE_LOOP('',(#10868,#10869,#10870,#10871));
#2553=EDGE_LOOP('',(#10872,#10873,#10874,#10875));
#2554=EDGE_LOOP('',(#10876,#10877,#10878,#10879));
#2555=EDGE_LOOP('',(#10880));
#2556=EDGE_LOOP('',(#10881,#10882,#10883,#10884));
#2557=EDGE_LOOP('',(#10885,#10886,#10887,#10888));
#2558=EDGE_LOOP('',(#10889,#10890,#10891,#10892));
#2559=EDGE_LOOP('',(#10893,#10894,#10895,#10896,#10897,#10898,#10899,#10900));
#2560=EDGE_LOOP('',(#10901,#10902,#10903,#10904,#10905,#10906,#10907,#10908));
#2561=EDGE_LOOP('',(#10909,#10910,#10911,#10912,#10913));
#2562=EDGE_LOOP('',(#10914,#10915,#10916,#10917,#10918,#10919));
#2563=EDGE_LOOP('',(#10920));
#2564=EDGE_LOOP('',(#10921,#10922,#10923,#10924,#10925,#10926));
#2565=EDGE_LOOP('',(#10927,#10928,#10929,#10930,#10931));
#2566=EDGE_LOOP('',(#10932));
#2567=EDGE_LOOP('',(#10933,#10934,#10935,#10936));
#2568=EDGE_LOOP('',(#10937));
#2569=EDGE_LOOP('',(#10938,#10939,#10940,#10941));
#2570=EDGE_LOOP('',(#10942,#10943,#10944,#10945));
#2571=EDGE_LOOP('',(#10946,#10947,#10948,#10949));
#2572=EDGE_LOOP('',(#10950));
#2573=EDGE_LOOP('',(#10951,#10952,#10953,#10954));
#2574=EDGE_LOOP('',(#10955,#10956,#10957,#10958));
#2575=EDGE_LOOP('',(#10959,#10960,#10961,#10962));
#2576=EDGE_LOOP('',(#10963,#10964,#10965,#10966));
#2577=EDGE_LOOP('',(#10967,#10968,#10969,#10970));
#2578=EDGE_LOOP('',(#10971,#10972,#10973,#10974));
#2579=EDGE_LOOP('',(#10975,#10976,#10977,#10978));
#2580=EDGE_LOOP('',(#10979,#10980,#10981,#10982));
#2581=EDGE_LOOP('',(#10983,#10984,#10985,#10986));
#2582=EDGE_LOOP('',(#10987,#10988,#10989,#10990));
#2583=EDGE_LOOP('',(#10991,#10992,#10993,#10994));
#2584=EDGE_LOOP('',(#10995,#10996,#10997,#10998));
#2585=EDGE_LOOP('',(#10999,#11000,#11001,#11002));
#2586=EDGE_LOOP('',(#11003,#11004,#11005,#11006));
#2587=EDGE_LOOP('',(#11007,#11008,#11009,#11010));
#2588=EDGE_LOOP('',(#11011,#11012,#11013,#11014));
#2589=EDGE_LOOP('',(#11015,#11016,#11017,#11018));
#2590=EDGE_LOOP('',(#11019,#11020,#11021,#11022));
#2591=EDGE_LOOP('',(#11023,#11024,#11025,#11026));
#2592=EDGE_LOOP('',(#11027,#11028,#11029,#11030));
#2593=EDGE_LOOP('',(#11031,#11032,#11033,#11034));
#2594=EDGE_LOOP('',(#11035,#11036,#11037,#11038));
#2595=EDGE_LOOP('',(#11039,#11040,#11041,#11042));
#2596=EDGE_LOOP('',(#11043,#11044,#11045,#11046));
#2597=EDGE_LOOP('',(#11047,#11048,#11049,#11050));
#2598=EDGE_LOOP('',(#11051,#11052,#11053,#11054));
#2599=EDGE_LOOP('',(#11055,#11056,#11057,#11058));
#2600=EDGE_LOOP('',(#11059,#11060,#11061,#11062));
#2601=EDGE_LOOP('',(#11063,#11064,#11065,#11066));
#2602=EDGE_LOOP('',(#11067,#11068,#11069,#11070));
#2603=EDGE_LOOP('',(#11071,#11072,#11073,#11074));
#2604=EDGE_LOOP('',(#11075,#11076,#11077,#11078));
#2605=EDGE_LOOP('',(#11079,#11080,#11081,#11082));
#2606=EDGE_LOOP('',(#11083,#11084,#11085,#11086));
#2607=EDGE_LOOP('',(#11087,#11088,#11089,#11090));
#2608=EDGE_LOOP('',(#11091,#11092,#11093,#11094));
#2609=EDGE_LOOP('',(#11095,#11096,#11097,#11098));
#2610=EDGE_LOOP('',(#11099,#11100,#11101,#11102));
#2611=EDGE_LOOP('',(#11103,#11104,#11105,#11106));
#2612=EDGE_LOOP('',(#11107,#11108,#11109,#11110));
#2613=EDGE_LOOP('',(#11111,#11112,#11113,#11114));
#2614=EDGE_LOOP('',(#11115,#11116,#11117,#11118));
#2615=EDGE_LOOP('',(#11119,#11120,#11121,#11122));
#2616=EDGE_LOOP('',(#11123,#11124,#11125,#11126));
#2617=EDGE_LOOP('',(#11127,#11128,#11129,#11130));
#2618=EDGE_LOOP('',(#11131,#11132,#11133,#11134));
#2619=EDGE_LOOP('',(#11135,#11136,#11137,#11138));
#2620=EDGE_LOOP('',(#11139,#11140,#11141,#11142));
#2621=EDGE_LOOP('',(#11143,#11144,#11145,#11146));
#2622=EDGE_LOOP('',(#11147,#11148,#11149,#11150));
#2623=EDGE_LOOP('',(#11151,#11152,#11153,#11154,#11155,#11156,#11157,#11158,
#11159,#11160,#11161,#11162,#11163,#11164,#11165,#11166,#11167,#11168,#11169,
#11170,#11171,#11172,#11173,#11174,#11175,#11176,#11177,#11178,#11179,#11180,
#11181,#11182,#11183,#11184,#11185,#11186,#11187,#11188,#11189,#11190,#11191,
#11192,#11193,#11194,#11195,#11196,#11197,#11198,#11199,#11200));
#2624=EDGE_LOOP('',(#11201,#11202,#11203,#11204,#11205,#11206,#11207,#11208,
#11209,#11210,#11211,#11212,#11213,#11214,#11215,#11216,#11217,#11218,#11219,
#11220,#11221,#11222,#11223,#11224,#11225,#11226,#11227,#11228,#11229,#11230,
#11231,#11232,#11233,#11234,#11235,#11236,#11237,#11238,#11239,#11240,#11241,
#11242,#11243,#11244,#11245,#11246,#11247,#11248,#11249,#11250));
#2625=EDGE_LOOP('',(#11251,#11252,#11253,#11254));
#2626=EDGE_LOOP('',(#11255,#11256,#11257,#11258));
#2627=EDGE_LOOP('',(#11259,#11260,#11261,#11262));
#2628=EDGE_LOOP('',(#11263,#11264,#11265,#11266));
#2629=EDGE_LOOP('',(#11267,#11268,#11269,#11270));
#2630=EDGE_LOOP('',(#11271,#11272,#11273,#11274));
#2631=EDGE_LOOP('',(#11275,#11276,#11277,#11278));
#2632=EDGE_LOOP('',(#11279,#11280,#11281,#11282));
#2633=EDGE_LOOP('',(#11283,#11284,#11285,#11286));
#2634=EDGE_LOOP('',(#11287,#11288,#11289,#11290));
#2635=EDGE_LOOP('',(#11291,#11292,#11293,#11294));
#2636=EDGE_LOOP('',(#11295,#11296,#11297,#11298));
#2637=EDGE_LOOP('',(#11299,#11300,#11301,#11302,#11303,#11304,#11305,#11306));
#2638=EDGE_LOOP('',(#11307,#11308,#11309,#11310,#11311,#11312,#11313,#11314));
#2639=EDGE_LOOP('',(#11315,#11316,#11317,#11318));
#2640=EDGE_LOOP('',(#11319,#11320,#11321,#11322));
#2641=EDGE_LOOP('',(#11323,#11324,#11325,#11326));
#2642=EDGE_LOOP('',(#11327,#11328,#11329,#11330));
#2643=EDGE_LOOP('',(#11331,#11332,#11333,#11334));
#2644=EDGE_LOOP('',(#11335,#11336,#11337,#11338));
#2645=EDGE_LOOP('',(#11339,#11340,#11341,#11342));
#2646=EDGE_LOOP('',(#11343,#11344,#11345,#11346));
#2647=EDGE_LOOP('',(#11347,#11348,#11349,#11350));
#2648=EDGE_LOOP('',(#11351,#11352,#11353,#11354));
#2649=EDGE_LOOP('',(#11355,#11356,#11357,#11358));
#2650=EDGE_LOOP('',(#11359,#11360,#11361,#11362));
#2651=EDGE_LOOP('',(#11363,#11364,#11365,#11366,#11367,#11368,#11369,#11370));
#2652=EDGE_LOOP('',(#11371,#11372,#11373,#11374,#11375,#11376,#11377,#11378));
#2653=EDGE_LOOP('',(#11379,#11380,#11381,#11382));
#2654=EDGE_LOOP('',(#11383,#11384,#11385,#11386));
#2655=EDGE_LOOP('',(#11387,#11388,#11389,#11390));
#2656=EDGE_LOOP('',(#11391,#11392,#11393,#11394));
#2657=EDGE_LOOP('',(#11395,#11396,#11397,#11398));
#2658=EDGE_LOOP('',(#11399,#11400,#11401,#11402));
#2659=EDGE_LOOP('',(#11403,#11404,#11405,#11406));
#2660=EDGE_LOOP('',(#11407,#11408,#11409,#11410));
#2661=EDGE_LOOP('',(#11411,#11412,#11413,#11414,#11415,#11416));
#2662=EDGE_LOOP('',(#11417,#11418,#11419,#11420,#11421,#11422,#11423,#11424,
#11425,#11426));
#2663=EDGE_LOOP('',(#11427,#11428,#11429,#11430,#11431,#11432));
#2664=EDGE_LOOP('',(#11433,#11434,#11435,#11436,#11437,#11438,#11439,#11440,
#11441,#11442));
#2665=EDGE_LOOP('',(#11443,#11444,#11445,#11446));
#2666=EDGE_LOOP('',(#11447,#11448,#11449,#11450));
#2667=EDGE_LOOP('',(#11451,#11452,#11453,#11454));
#2668=EDGE_LOOP('',(#11455,#11456,#11457,#11458));
#2669=EDGE_LOOP('',(#11459,#11460,#11461,#11462));
#2670=EDGE_LOOP('',(#11463,#11464,#11465,#11466));
#2671=EDGE_LOOP('',(#11467,#11468,#11469,#11470));
#2672=EDGE_LOOP('',(#11471,#11472,#11473,#11474,#11475,#11476));
#2673=EDGE_LOOP('',(#11477,#11478,#11479,#11480,#11481,#11482,#11483,#11484,
#11485,#11486));
#2674=EDGE_LOOP('',(#11487,#11488,#11489,#11490));
#2675=EDGE_LOOP('',(#11491,#11492,#11493,#11494));
#2676=EDGE_LOOP('',(#11495,#11496,#11497,#11498));
#2677=EDGE_LOOP('',(#11499,#11500,#11501,#11502));
#2678=EDGE_LOOP('',(#11503,#11504,#11505,#11506));
#2679=EDGE_LOOP('',(#11507,#11508,#11509,#11510));
#2680=EDGE_LOOP('',(#11511,#11512,#11513,#11514));
#2681=EDGE_LOOP('',(#11515,#11516,#11517,#11518,#11519,#11520));
#2682=EDGE_LOOP('',(#11521,#11522,#11523,#11524,#11525,#11526));
#2683=EDGE_LOOP('',(#11527,#11528,#11529,#11530,#11531,#11532,#11533,#11534,
#11535,#11536));
#2684=EDGE_LOOP('',(#11537,#11538,#11539,#11540));
#2685=EDGE_LOOP('',(#11541,#11542,#11543,#11544));
#2686=EDGE_LOOP('',(#11545,#11546,#11547,#11548));
#2687=EDGE_LOOP('',(#11549,#11550,#11551,#11552));
#2688=EDGE_LOOP('',(#11553,#11554,#11555,#11556));
#2689=EDGE_LOOP('',(#11557,#11558,#11559,#11560));
#2690=EDGE_LOOP('',(#11561,#11562,#11563,#11564));
#2691=EDGE_LOOP('',(#11565,#11566,#11567,#11568));
#2692=EDGE_LOOP('',(#11569,#11570,#11571,#11572,#11573,#11574,#11575,#11576,
#11577,#11578,#11579,#11580,#11581,#11582,#11583,#11584));
#2693=EDGE_LOOP('',(#11585,#11586,#11587,#11588,#11589,#11590,#11591,#11592));
#2694=EDGE_LOOP('',(#11593,#11594,#11595,#11596));
#2695=EDGE_LOOP('',(#11597,#11598,#11599,#11600));
#2696=EDGE_LOOP('',(#11601,#11602,#11603,#11604));
#2697=EDGE_LOOP('',(#11605,#11606,#11607,#11608));
#2698=EDGE_LOOP('',(#11609,#11610,#11611,#11612));
#2699=EDGE_LOOP('',(#11613,#11614,#11615,#11616));
#2700=EDGE_LOOP('',(#11617,#11618,#11619,#11620));
#2701=EDGE_LOOP('',(#11621,#11622,#11623,#11624,#11625,#11626));
#2702=EDGE_LOOP('',(#11627,#11628,#11629,#11630));
#2703=EDGE_LOOP('',(#11631,#11632,#11633,#11634));
#2704=EDGE_LOOP('',(#11635,#11636,#11637,#11638));
#2705=EDGE_LOOP('',(#11639,#11640,#11641,#11642));
#2706=EDGE_LOOP('',(#11643,#11644,#11645,#11646));
#2707=EDGE_LOOP('',(#11647,#11648,#11649,#11650));
#2708=EDGE_LOOP('',(#11651,#11652,#11653,#11654));
#2709=EDGE_LOOP('',(#11655,#11656,#11657,#11658,#11659,#11660));
#2710=EDGE_LOOP('',(#11661,#11662,#11663,#11664,#11665,#11666));
#2711=EDGE_LOOP('',(#11667,#11668,#11669,#11670));
#2712=EDGE_LOOP('',(#11671,#11672,#11673,#11674));
#2713=EDGE_LOOP('',(#11675,#11676,#11677,#11678));
#2714=EDGE_LOOP('',(#11679,#11680,#11681,#11682));
#2715=EDGE_LOOP('',(#11683,#11684,#11685,#11686));
#2716=EDGE_LOOP('',(#11687,#11688,#11689,#11690));
#2717=EDGE_LOOP('',(#11691,#11692,#11693,#11694));
#2718=EDGE_LOOP('',(#11695,#11696,#11697,#11698));
#2719=EDGE_LOOP('',(#11699,#11700,#11701,#11702,#11703,#11704));
#2720=EDGE_LOOP('',(#11705,#11706,#11707,#11708));
#2721=EDGE_LOOP('',(#11709,#11710,#11711,#11712));
#2722=EDGE_LOOP('',(#11713,#11714,#11715,#11716));
#2723=EDGE_LOOP('',(#11717,#11718,#11719,#11720));
#2724=EDGE_LOOP('',(#11721,#11722,#11723,#11724));
#2725=EDGE_LOOP('',(#11725,#11726,#11727,#11728));
#2726=EDGE_LOOP('',(#11729,#11730,#11731,#11732));
#2727=EDGE_LOOP('',(#11733,#11734,#11735,#11736,#11737,#11738,#11739,#11740,
#11741,#11742,#11743,#11744,#11745,#11746,#11747,#11748,#11749,#11750,#11751,
#11752,#11753,#11754));
#2728=EDGE_LOOP('',(#11755,#11756,#11757,#11758));
#2729=EDGE_LOOP('',(#11759,#11760,#11761,#11762));
#2730=EDGE_LOOP('',(#11763,#11764,#11765,#11766));
#2731=EDGE_LOOP('',(#11767,#11768,#11769,#11770));
#2732=EDGE_LOOP('',(#11771,#11772,#11773));
#2733=EDGE_LOOP('',(#11774,#11775,#11776,#11777,#11778));
#2734=EDGE_LOOP('',(#11779,#11780,#11781,#11782,#11783));
#2735=EDGE_LOOP('',(#11784,#11785,#11786,#11787));
#2736=EDGE_LOOP('',(#11788,#11789,#11790,#11791));
#2737=EDGE_LOOP('',(#11792,#11793,#11794,#11795,#11796));
#2738=EDGE_LOOP('',(#11797,#11798,#11799,#11800,#11801));
#2739=EDGE_LOOP('',(#11802,#11803,#11804,#11805));
#2740=EDGE_LOOP('',(#11806,#11807,#11808,#11809));
#2741=EDGE_LOOP('',(#11810,#11811,#11812,#11813));
#2742=EDGE_LOOP('',(#11814,#11815,#11816,#11817));
#2743=EDGE_LOOP('',(#11818,#11819,#11820,#11821));
#2744=EDGE_LOOP('',(#11822,#11823,#11824,#11825));
#2745=EDGE_LOOP('',(#11826,#11827,#11828,#11829));
#2746=EDGE_LOOP('',(#11830,#11831,#11832,#11833));
#2747=EDGE_LOOP('',(#11834,#11835,#11836,#11837,#11838,#11839));
#2748=EDGE_LOOP('',(#11840,#11841,#11842,#11843,#11844,#11845));
#2749=EDGE_LOOP('',(#11846,#11847,#11848,#11849,#11850,#11851,#11852,#11853,
#11854,#11855));
#2750=EDGE_LOOP('',(#11856,#11857,#11858,#11859));
#2751=EDGE_LOOP('',(#11860,#11861,#11862,#11863));
#2752=EDGE_LOOP('',(#11864,#11865,#11866,#11867));
#2753=EDGE_LOOP('',(#11868,#11869,#11870,#11871));
#2754=EDGE_LOOP('',(#11872,#11873,#11874,#11875));
#2755=EDGE_LOOP('',(#11876,#11877,#11878,#11879));
#2756=EDGE_LOOP('',(#11880,#11881,#11882,#11883));
#2757=EDGE_LOOP('',(#11884,#11885,#11886,#11887,#11888,#11889,#11890,#11891,
#11892,#11893,#11894,#11895,#11896,#11897,#11898,#11899));
#2758=EDGE_LOOP('',(#11900,#11901,#11902));
#2759=EDGE_LOOP('',(#11903,#11904,#11905,#11906,#11907));
#2760=EDGE_LOOP('',(#11908,#11909,#11910,#11911));
#2761=EDGE_LOOP('',(#11912,#11913,#11914,#11915));
#2762=EDGE_LOOP('',(#11916,#11917,#11918,#11919));
#2763=EDGE_LOOP('',(#11920,#11921,#11922,#11923));
#2764=EDGE_LOOP('',(#11924,#11925,#11926,#11927));
#2765=EDGE_LOOP('',(#11928,#11929,#11930,#11931));
#2766=EDGE_LOOP('',(#11932,#11933,#11934,#11935));
#2767=EDGE_LOOP('',(#11936,#11937,#11938,#11939));
#2768=EDGE_LOOP('',(#11940,#11941,#11942,#11943));
#2769=EDGE_LOOP('',(#11944,#11945,#11946,#11947,#11948));
#2770=EDGE_LOOP('',(#11949,#11950,#11951,#11952));
#2771=EDGE_LOOP('',(#11953,#11954,#11955,#11956,#11957,#11958,#11959,#11960,
#11961,#11962));
#2772=EDGE_LOOP('',(#11963,#11964,#11965,#11966,#11967,#11968));
#2773=EDGE_LOOP('',(#11969,#11970,#11971,#11972,#11973,#11974,#11975,#11976,
#11977,#11978));
#2774=EDGE_LOOP('',(#11979,#11980,#11981,#11982));
#2775=EDGE_LOOP('',(#11983,#11984,#11985,#11986));
#2776=EDGE_LOOP('',(#11987,#11988,#11989,#11990));
#2777=EDGE_LOOP('',(#11991,#11992,#11993,#11994));
#2778=EDGE_LOOP('',(#11995,#11996,#11997,#11998));
#2779=EDGE_LOOP('',(#11999,#12000,#12001,#12002));
#2780=EDGE_LOOP('',(#12003,#12004,#12005,#12006));
#2781=EDGE_LOOP('',(#12007,#12008,#12009,#12010));
#2782=EDGE_LOOP('',(#12011,#12012,#12013,#12014));
#2783=EDGE_LOOP('',(#12015,#12016,#12017,#12018,#12019,#12020));
#2784=EDGE_LOOP('',(#12021,#12022,#12023,#12024,#12025,#12026));
#2785=EDGE_LOOP('',(#12027,#12028,#12029,#12030,#12031,#12032,#12033,#12034,
#12035,#12036));
#2786=EDGE_LOOP('',(#12037,#12038,#12039,#12040));
#2787=EDGE_LOOP('',(#12041,#12042,#12043,#12044));
#2788=EDGE_LOOP('',(#12045,#12046,#12047,#12048));
#2789=EDGE_LOOP('',(#12049,#12050,#12051,#12052));
#2790=EDGE_LOOP('',(#12053,#12054,#12055,#12056));
#2791=EDGE_LOOP('',(#12057,#12058,#12059,#12060));
#2792=EDGE_LOOP('',(#12061,#12062,#12063,#12064));
#2793=EDGE_LOOP('',(#12065,#12066,#12067,#12068,#12069,#12070));
#2794=EDGE_LOOP('',(#12071,#12072,#12073,#12074,#12075,#12076));
#2795=EDGE_LOOP('',(#12077,#12078,#12079,#12080,#12081,#12082,#12083,#12084,
#12085,#12086));
#2796=EDGE_LOOP('',(#12087,#12088,#12089,#12090));
#2797=EDGE_LOOP('',(#12091,#12092,#12093,#12094));
#2798=EDGE_LOOP('',(#12095,#12096,#12097,#12098));
#2799=EDGE_LOOP('',(#12099,#12100,#12101,#12102));
#2800=EDGE_LOOP('',(#12103,#12104,#12105,#12106,#12107,#12108,#12109,#12110));
#2801=EDGE_LOOP('',(#12111,#12112,#12113,#12114));
#2802=EDGE_LOOP('',(#12115,#12116,#12117,#12118));
#2803=EDGE_LOOP('',(#12119,#12120,#12121,#12122,#12123,#12124,#12125,#12126,
#12127,#12128));
#2804=EDGE_LOOP('',(#12129));
#2805=EDGE_LOOP('',(#12130,#12131,#12132,#12133));
#2806=EDGE_LOOP('',(#12134,#12135,#12136,#12137,#12138,#12139,#12140,#12141,
#12142,#12143,#12144,#12145,#12146,#12147,#12148,#12149,#12150,#12151,#12152,
#12153,#12154,#12155,#12156,#12157,#12158,#12159,#12160,#12161,#12162,#12163,
#12164,#12165,#12166,#12167,#12168,#12169,#12170,#12171,#12172,#12173,#12174,
#12175,#12176,#12177,#12178,#12179,#12180,#12181,#12182,#12183,#12184,#12185,
#12186,#12187,#12188,#12189,#12190,#12191,#12192,#12193));
#2807=EDGE_LOOP('',(#12194));
#2808=EDGE_LOOP('',(#12195,#12196,#12197,#12198));
#2809=EDGE_LOOP('',(#12199,#12200,#12201,#12202));
#2810=EDGE_LOOP('',(#12203,#12204,#12205,#12206));
#2811=EDGE_LOOP('',(#12207,#12208,#12209,#12210));
#2812=EDGE_LOOP('',(#12211,#12212,#12213,#12214));
#2813=EDGE_LOOP('',(#12215,#12216,#12217,#12218));
#2814=EDGE_LOOP('',(#12219,#12220,#12221));
#2815=EDGE_LOOP('',(#12222,#12223,#12224,#12225,#12226));
#2816=EDGE_LOOP('',(#12227,#12228,#12229));
#2817=EDGE_LOOP('',(#12230,#12231,#12232,#12233));
#2818=EDGE_LOOP('',(#12234,#12235,#12236));
#2819=EDGE_LOOP('',(#12237,#12238,#12239,#12240));
#2820=EDGE_LOOP('',(#12241,#12242,#12243,#12244,#12245));
#2821=EDGE_LOOP('',(#12246,#12247,#12248,#12249));
#2822=EDGE_LOOP('',(#12250,#12251,#12252,#12253));
#2823=EDGE_LOOP('',(#12254,#12255,#12256,#12257));
#2824=EDGE_LOOP('',(#12258,#12259,#12260,#12261,#12262,#12263,#12264,#12265));
#2825=EDGE_LOOP('',(#12266,#12267,#12268,#12269,#12270,#12271,#12272,#12273));
#2826=EDGE_LOOP('',(#12274,#12275,#12276,#12277,#12278,#12279,#12280,#12281));
#2827=EDGE_LOOP('',(#12282,#12283,#12284,#12285,#12286));
#2828=EDGE_LOOP('',(#12287,#12288,#12289,#12290,#12291));
#2829=EDGE_LOOP('',(#12292,#12293,#12294,#12295));
#2830=EDGE_LOOP('',(#12296,#12297,#12298,#12299));
#2831=EDGE_LOOP('',(#12300,#12301,#12302,#12303));
#2832=EDGE_LOOP('',(#12304,#12305,#12306,#12307));
#2833=EDGE_LOOP('',(#12308,#12309,#12310,#12311));
#2834=EDGE_LOOP('',(#12312,#12313,#12314,#12315));
#2835=EDGE_LOOP('',(#12316,#12317,#12318,#12319));
#2836=EDGE_LOOP('',(#12320,#12321,#12322,#12323));
#2837=EDGE_LOOP('',(#12324,#12325,#12326,#12327));
#2838=EDGE_LOOP('',(#12328,#12329,#12330,#12331));
#2839=EDGE_LOOP('',(#12332,#12333,#12334,#12335));
#2840=EDGE_LOOP('',(#12336,#12337,#12338,#12339));
#2841=EDGE_LOOP('',(#12340,#12341,#12342));
#2842=EDGE_LOOP('',(#12343,#12344,#12345));
#2843=EDGE_LOOP('',(#12346,#12347,#12348,#12349));
#2844=EDGE_LOOP('',(#12350,#12351,#12352));
#2845=EDGE_LOOP('',(#12353,#12354,#12355,#12356));
#2846=EDGE_LOOP('',(#12357,#12358,#12359));
#2847=EDGE_LOOP('',(#12360,#12361,#12362,#12363));
#2848=EDGE_LOOP('',(#12364,#12365,#12366));
#2849=EDGE_LOOP('',(#12367,#12368,#12369,#12370,#12371));
#2850=EDGE_LOOP('',(#12372,#12373,#12374,#12375));
#2851=EDGE_LOOP('',(#12376,#12377,#12378,#12379));
#2852=EDGE_LOOP('',(#12380,#12381,#12382,#12383,#12384));
#2853=EDGE_LOOP('',(#12385,#12386,#12387,#12388));
#2854=EDGE_LOOP('',(#12389,#12390,#12391,#12392));
#2855=EDGE_LOOP('',(#12393,#12394,#12395,#12396));
#2856=EDGE_LOOP('',(#12397,#12398,#12399,#12400));
#2857=EDGE_LOOP('',(#12401,#12402,#12403,#12404,#12405,#12406,#12407,#12408));
#2858=EDGE_LOOP('',(#12409,#12410,#12411,#12412,#12413,#12414,#12415,#12416));
#2859=EDGE_LOOP('',(#12417,#12418,#12419,#12420,#12421,#12422,#12423,#12424));
#2860=EDGE_LOOP('',(#12425,#12426,#12427,#12428,#12429,#12430,#12431,#12432));
#2861=EDGE_LOOP('',(#12433,#12434,#12435,#12436,#12437,#12438,#12439,#12440));
#2862=EDGE_LOOP('',(#12441,#12442,#12443,#12444));
#2863=EDGE_LOOP('',(#12445,#12446,#12447,#12448));
#2864=EDGE_LOOP('',(#12449,#12450,#12451,#12452));
#2865=EDGE_LOOP('',(#12453,#12454,#12455,#12456,#12457));
#2866=EDGE_LOOP('',(#12458,#12459,#12460,#12461,#12462));
#2867=EDGE_LOOP('',(#12463,#12464,#12465,#12466,#12467,#12468,#12469,#12470));
#2868=EDGE_LOOP('',(#12471,#12472,#12473,#12474));
#2869=EDGE_LOOP('',(#12475,#12476,#12477,#12478,#12479));
#2870=EDGE_LOOP('',(#12480,#12481,#12482,#12483,#12484));
#2871=EDGE_LOOP('',(#12485,#12486,#12487,#12488));
#2872=EDGE_LOOP('',(#12489,#12490,#12491,#12492,#12493));
#2873=EDGE_LOOP('',(#12494,#12495,#12496,#12497,#12498));
#2874=EDGE_LOOP('',(#12499,#12500,#12501,#12502));
#2875=EDGE_LOOP('',(#12503,#12504,#12505,#12506,#12507));
#2876=EDGE_LOOP('',(#12508,#12509,#12510,#12511,#12512));
#2877=EDGE_LOOP('',(#12513,#12514,#12515,#12516));
#2878=EDGE_LOOP('',(#12517,#12518,#12519,#12520,#12521));
#2879=EDGE_LOOP('',(#12522,#12523,#12524,#12525,#12526));
#2880=EDGE_LOOP('',(#12527,#12528,#12529,#12530));
#2881=EDGE_LOOP('',(#12531,#12532,#12533,#12534,#12535));
#2882=EDGE_LOOP('',(#12536,#12537,#12538,#12539,#12540));
#2883=EDGE_LOOP('',(#12541,#12542,#12543,#12544));
#2884=EDGE_LOOP('',(#12545,#12546,#12547,#12548,#12549));
#2885=EDGE_LOOP('',(#12550,#12551,#12552,#12553,#12554));
#2886=EDGE_LOOP('',(#12555,#12556,#12557,#12558));
#2887=EDGE_LOOP('',(#12559,#12560,#12561,#12562,#12563));
#2888=EDGE_LOOP('',(#12564,#12565,#12566,#12567,#12568));
#2889=EDGE_LOOP('',(#12569,#12570,#12571,#12572));
#2890=EDGE_LOOP('',(#12573,#12574,#12575,#12576,#12577));
#2891=EDGE_LOOP('',(#12578,#12579,#12580,#12581,#12582));
#2892=EDGE_LOOP('',(#12583,#12584,#12585,#12586,#12587));
#2893=EDGE_LOOP('',(#12588,#12589,#12590,#12591,#12592));
#2894=EDGE_LOOP('',(#12593,#12594,#12595,#12596));
#2895=EDGE_LOOP('',(#12597,#12598,#12599,#12600,#12601,#12602,#12603,#12604));
#2896=LINE('',#18382,#4207);
#2897=LINE('',#18384,#4208);
#2898=LINE('',#18386,#4209);
#2899=LINE('',#18387,#4210);
#2900=LINE('',#18391,#4211);
#2901=LINE('',#18397,#4212);
#2902=LINE('',#18398,#4213);
#2903=LINE('',#18399,#4214);
#2904=LINE('',#18403,#4215);
#2905=LINE('',#18409,#4216);
#2906=LINE('',#18410,#4217);
#2907=LINE('',#18411,#4218);
#2908=LINE('',#18415,#4219);
#2909=LINE('',#18421,#4220);
#2910=LINE('',#18422,#4221);
#2911=LINE('',#18423,#4222);
#2912=LINE('',#18429,#4223);
#2913=LINE('',#18432,#4224);
#2914=LINE('',#18435,#4225);
#2915=LINE('',#18436,#4226);
#2916=LINE('',#18441,#4227);
#2917=LINE('',#18445,#4228);
#2918=LINE('',#18446,#4229);
#2919=LINE('',#18450,#4230);
#2920=LINE('',#18454,#4231);
#2921=LINE('',#18458,#4232);
#2922=LINE('',#18462,#4233);
#2923=LINE('',#18466,#4234);
#2924=LINE('',#18468,#4235);
#2925=LINE('',#18469,#4236);
#2926=LINE('',#18472,#4237);
#2927=LINE('',#18476,#4238);
#2928=LINE('',#18477,#4239);
#2929=LINE('',#18480,#4240);
#2930=LINE('',#18484,#4241);
#2931=LINE('',#18485,#4242);
#2932=LINE('',#18488,#4243);
#2933=LINE('',#18492,#4244);
#2934=LINE('',#18493,#4245);
#2935=LINE('',#18498,#4246);
#2936=LINE('',#18501,#4247);
#2937=LINE('',#18504,#4248);
#2938=LINE('',#18505,#4249);
#2939=LINE('',#18508,#4250);
#2940=LINE('',#18512,#4251);
#2941=LINE('',#18513,#4252);
#2942=LINE('',#18516,#4253);
#2943=LINE('',#18518,#4254);
#2944=LINE('',#18519,#4255);
#2945=LINE('',#18522,#4256);
#2946=LINE('',#18527,#4257);
#2947=LINE('',#18528,#4258);
#2948=LINE('',#18529,#4259);
#2949=LINE('',#18533,#4260);
#2950=LINE('',#18539,#4261);
#2951=LINE('',#18540,#4262);
#2952=LINE('',#18541,#4263);
#2953=LINE('',#18544,#4264);
#2954=LINE('',#18549,#4265);
#2955=LINE('',#18550,#4266);
#2956=LINE('',#18554,#4267);
#2957=LINE('',#18558,#4268);
#2958=LINE('',#18562,#4269);
#2959=LINE('',#18566,#4270);
#2960=LINE('',#18570,#4271);
#2961=LINE('',#18573,#4272);
#2962=LINE('',#18574,#4273);
#2963=LINE('',#18576,#4274);
#2964=LINE('',#18579,#4275);
#2965=LINE('',#18580,#4276);
#2966=LINE('',#18583,#4277);
#2967=LINE('',#18587,#4278);
#2968=LINE('',#18588,#4279);
#2969=LINE('',#18590,#4280);
#2970=LINE('',#18593,#4281);
#2971=LINE('',#18596,#4282);
#2972=LINE('',#18600,#4283);
#2973=LINE('',#18602,#4284);
#2974=LINE('',#18604,#4285);
#2975=LINE('',#18607,#4286);
#2976=LINE('',#18609,#4287);
#2977=LINE('',#18774,#4288);
#2978=LINE('',#18953,#4289);
#2979=LINE('',#18986,#4290);
#2980=LINE('',#18996,#4291);
#2981=LINE('',#19000,#4292);
#2982=LINE('',#19058,#4293);
#2983=LINE('',#19091,#4294);
#2984=LINE('',#19182,#4295);
#2985=LINE('',#19185,#4296);
#2986=LINE('',#19187,#4297);
#2987=LINE('',#19189,#4298);
#2988=LINE('',#19191,#4299);
#2989=LINE('',#19193,#4300);
#2990=LINE('',#19194,#4301);
#2991=LINE('',#19197,#4302);
#2992=LINE('',#19491,#4303);
#2993=LINE('',#19616,#4304);
#2994=LINE('',#19620,#4305);
#2995=LINE('',#19624,#4306);
#2996=LINE('',#19682,#4307);
#2997=LINE('',#19715,#4308);
#2998=LINE('',#19719,#4309);
#2999=LINE('',#19722,#4310);
#3000=LINE('',#20061,#4311);
#3001=LINE('',#20094,#4312);
#3002=LINE('',#20104,#4313);
#3003=LINE('',#20108,#4314);
#3004=LINE('',#20166,#4315);
#3005=LINE('',#20288,#4316);
#3006=LINE('',#20290,#4317);
#3007=LINE('',#20399,#4318);
#3008=LINE('',#20464,#4319);
#3009=LINE('',#20467,#4320);
#3010=LINE('',#20470,#4321);
#3011=LINE('',#20522,#4322);
#3012=LINE('',#20545,#4323);
#3013=LINE('',#20549,#4324);
#3014=LINE('',#20552,#4325);
#3015=LINE('',#20555,#4326);
#3016=LINE('',#20564,#4327);
#3017=LINE('',#20579,#4328);
#3018=LINE('',#20587,#4329);
#3019=LINE('',#20597,#4330);
#3020=LINE('',#20600,#4331);
#3021=LINE('',#20615,#4332);
#3022=LINE('',#20623,#4333);
#3023=LINE('',#20626,#4334);
#3024=LINE('',#20628,#4335);
#3025=LINE('',#20755,#4336);
#3026=LINE('',#20880,#4337);
#3027=LINE('',#20918,#4338);
#3028=LINE('',#20929,#4339);
#3029=LINE('',#20930,#4340);
#3030=LINE('',#20931,#4341);
#3031=LINE('',#20970,#4342);
#3032=LINE('',#21025,#4343);
#3033=LINE('',#21028,#4344);
#3034=LINE('',#21029,#4345);
#3035=LINE('',#21032,#4346);
#3036=LINE('',#21088,#4347);
#3037=LINE('',#21090,#4348);
#3038=LINE('',#21092,#4349);
#3039=LINE('',#21094,#4350);
#3040=LINE('',#21096,#4351);
#3041=LINE('',#21097,#4352);
#3042=LINE('',#21174,#4353);
#3043=LINE('',#21281,#4354);
#3044=LINE('',#21284,#4355);
#3045=LINE('',#21285,#4356);
#3046=LINE('',#21318,#4357);
#3047=LINE('',#21373,#4358);
#3048=LINE('',#21376,#4359);
#3049=LINE('',#21377,#4360);
#3050=LINE('',#21583,#4361);
#3051=LINE('',#21609,#4362);
#3052=LINE('',#21618,#4363);
#3053=LINE('',#21619,#4364);
#3054=LINE('',#21896,#4365);
#3055=LINE('',#21929,#4366);
#3056=LINE('',#21938,#4367);
#3057=LINE('',#21940,#4368);
#3058=LINE('',#21941,#4369);
#3059=LINE('',#21979,#4370);
#3060=LINE('',#21981,#4371);
#3061=LINE('',#21983,#4372);
#3062=LINE('',#21985,#4373);
#3063=LINE('',#21986,#4374);
#3064=LINE('',#21989,#4375);
#3065=LINE('',#21996,#4376);
#3066=LINE('',#22000,#4377);
#3067=LINE('',#22005,#4378);
#3068=LINE('',#22007,#4379);
#3069=LINE('',#22009,#4380);
#3070=LINE('',#22010,#4381);
#3071=LINE('',#22014,#4382);
#3072=LINE('',#22018,#4383);
#3073=LINE('',#22020,#4384);
#3074=LINE('',#22022,#4385);
#3075=LINE('',#22023,#4386);
#3076=LINE('',#22027,#4387);
#3077=LINE('',#22029,#4388);
#3078=LINE('',#22031,#4389);
#3079=LINE('',#22032,#4390);
#3080=LINE('',#22036,#4391);
#3081=LINE('',#22042,#4392);
#3082=LINE('',#22043,#4393);
#3083=LINE('',#22044,#4394);
#3084=LINE('',#22047,#4395);
#3085=LINE('',#22052,#4396);
#3086=LINE('',#22053,#4397);
#3087=LINE('',#22057,#4398);
#3088=LINE('',#22063,#4399);
#3089=LINE('',#22064,#4400);
#3090=LINE('',#22065,#4401);
#3091=LINE('',#22071,#4402);
#3092=LINE('',#22075,#4403);
#3093=LINE('',#22076,#4404);
#3094=LINE('',#22079,#4405);
#3095=LINE('',#22083,#4406);
#3096=LINE('',#22084,#4407);
#3097=LINE('',#22090,#4408);
#3098=LINE('',#22094,#4409);
#3099=LINE('',#22098,#4410);
#3100=LINE('',#22101,#4411);
#3101=LINE('',#22104,#4412);
#3102=LINE('',#22105,#4413);
#3103=LINE('',#22109,#4414);
#3104=LINE('',#22110,#4415);
#3105=LINE('',#22113,#4416);
#3106=LINE('',#22117,#4417);
#3107=LINE('',#22118,#4418);
#3108=LINE('',#22121,#4419);
#3109=LINE('',#22125,#4420);
#3110=LINE('',#22126,#4421);
#3111=LINE('',#22128,#4422);
#3112=LINE('',#22133,#4423);
#3113=LINE('',#22135,#4424);
#3114=LINE('',#22136,#4425);
#3115=LINE('',#22139,#4426);
#3116=LINE('',#22143,#4427);
#3117=LINE('',#22144,#4428);
#3118=LINE('',#22149,#4429);
#3119=LINE('',#22151,#4430);
#3120=LINE('',#22152,#4431);
#3121=LINE('',#22155,#4432);
#3122=LINE('',#22159,#4433);
#3123=LINE('',#22160,#4434);
#3124=LINE('',#22163,#4435);
#3125=LINE('',#22167,#4436);
#3126=LINE('',#22168,#4437);
#3127=LINE('',#22172,#4438);
#3128=LINE('',#22178,#4439);
#3129=LINE('',#22179,#4440);
#3130=LINE('',#22180,#4441);
#3131=LINE('',#22187,#4442);
#3132=LINE('',#22191,#4443);
#3133=LINE('',#22195,#4444);
#3134=LINE('',#22199,#4445);
#3135=LINE('',#22202,#4446);
#3136=LINE('',#22203,#4447);
#3137=LINE('',#22205,#4448);
#3138=LINE('',#22207,#4449);
#3139=LINE('',#22210,#4450);
#3140=LINE('',#22214,#4451);
#3141=LINE('',#22215,#4452);
#3142=LINE('',#22217,#4453);
#3143=LINE('',#22220,#4454);
#3144=LINE('',#22223,#4455);
#3145=LINE('',#22225,#4456);
#3146=LINE('',#22228,#4457);
#3147=LINE('',#22230,#4458);
#3148=LINE('',#22237,#4459);
#3149=LINE('',#22242,#4460);
#3150=LINE('',#22244,#4461);
#3151=LINE('',#22246,#4462);
#3152=LINE('',#22247,#4463);
#3153=LINE('',#22261,#4464);
#3154=LINE('',#22264,#4465);
#3155=LINE('',#22269,#4466);
#3156=LINE('',#22272,#4467);
#3157=LINE('',#22277,#4468);
#3158=LINE('',#22280,#4469);
#3159=LINE('',#22285,#4470);
#3160=LINE('',#22288,#4471);
#3161=LINE('',#22293,#4472);
#3162=LINE('',#22296,#4473);
#3163=LINE('',#22301,#4474);
#3164=LINE('',#22306,#4475);
#3165=LINE('',#22311,#4476);
#3166=LINE('',#22313,#4477);
#3167=LINE('',#22315,#4478);
#3168=LINE('',#22316,#4479);
#3169=LINE('',#22332,#4480);
#3170=LINE('',#22335,#4481);
#3171=LINE('',#22337,#4482);
#3172=LINE('',#22338,#4483);
#3173=LINE('',#22342,#4484);
#3174=LINE('',#22348,#4485);
#3175=LINE('',#22349,#4486);
#3176=LINE('',#22350,#4487);
#3177=LINE('',#22354,#4488);
#3178=LINE('',#22360,#4489);
#3179=LINE('',#22361,#4490);
#3180=LINE('',#22362,#4491);
#3181=LINE('',#22365,#4492);
#3182=LINE('',#22370,#4493);
#3183=LINE('',#22371,#4494);
#3184=LINE('',#22378,#4495);
#3185=LINE('',#22384,#4496);
#3186=LINE('',#22388,#4497);
#3187=LINE('',#22392,#4498);
#3188=LINE('',#22396,#4499);
#3189=LINE('',#22400,#4500);
#3190=LINE('',#22405,#4501);
#3191=LINE('',#22408,#4502);
#3192=LINE('',#22413,#4503);
#3193=LINE('',#22416,#4504);
#3194=LINE('',#22421,#4505);
#3195=LINE('',#22424,#4506);
#3196=LINE('',#22429,#4507);
#3197=LINE('',#22432,#4508);
#3198=LINE('',#22437,#4509);
#3199=LINE('',#22440,#4510);
#3200=LINE('',#22445,#4511);
#3201=LINE('',#22449,#4512);
#3202=LINE('',#22453,#4513);
#3203=LINE('',#22455,#4514);
#3204=LINE('',#22457,#4515);
#3205=LINE('',#22458,#4516);
#3206=LINE('',#22472,#4517);
#3207=LINE('',#22474,#4518);
#3208=LINE('',#22476,#4519);
#3209=LINE('',#22478,#4520);
#3210=LINE('',#22480,#4521);
#3211=LINE('',#22482,#4522);
#3212=LINE('',#22485,#4523);
#3213=LINE('',#22487,#4524);
#3214=LINE('',#22488,#4525);
#3215=LINE('',#22491,#4526);
#3216=LINE('',#22495,#4527);
#3217=LINE('',#22496,#4528);
#3218=LINE('',#22499,#4529);
#3219=LINE('',#22503,#4530);
#3220=LINE('',#22504,#4531);
#3221=LINE('',#22506,#4532);
#3222=LINE('',#22509,#4533);
#3223=LINE('',#22515,#4534);
#3224=LINE('',#22518,#4535);
#3225=LINE('',#22522,#4536);
#3226=LINE('',#22523,#4537);
#3227=LINE('',#22537,#4538);
#3228=LINE('',#22539,#4539);
#3229=LINE('',#22541,#4540);
#3230=LINE('',#22543,#4541);
#3231=LINE('',#22545,#4542);
#3232=LINE('',#22547,#4543);
#3233=LINE('',#22550,#4544);
#3234=LINE('',#22552,#4545);
#3235=LINE('',#22553,#4546);
#3236=LINE('',#22556,#4547);
#3237=LINE('',#22560,#4548);
#3238=LINE('',#22561,#4549);
#3239=LINE('',#22565,#4550);
#3240=LINE('',#22571,#4551);
#3241=LINE('',#22572,#4552);
#3242=LINE('',#22573,#4553);
#3243=LINE('',#22577,#4554);
#3244=LINE('',#22582,#4555);
#3245=LINE('',#22583,#4556);
#3246=LINE('',#22584,#4557);
#3247=LINE('',#22588,#4558);
#3248=LINE('',#22592,#4559);
#3249=LINE('',#22596,#4560);
#3250=LINE('',#22600,#4561);
#3251=LINE('',#22604,#4562);
#3252=LINE('',#22607,#4563);
#3253=LINE('',#22608,#4564);
#3254=LINE('',#22610,#4565);
#3255=LINE('',#22612,#4566);
#3256=LINE('',#22615,#4567);
#3257=LINE('',#22619,#4568);
#3258=LINE('',#22620,#4569);
#3259=LINE('',#22623,#4570);
#3260=LINE('',#22626,#4571);
#3261=LINE('',#22627,#4572);
#3262=LINE('',#22630,#4573);
#3263=LINE('',#22632,#4574);
#3264=LINE('',#22634,#4575);
#3265=LINE('',#22637,#4576);
#3266=LINE('',#22639,#4577);
#3267=LINE('',#22804,#4578);
#3268=LINE('',#22983,#4579);
#3269=LINE('',#23006,#4580);
#3270=LINE('',#23014,#4581);
#3271=LINE('',#23018,#4582);
#3272=LINE('',#23076,#4583);
#3273=LINE('',#23109,#4584);
#3274=LINE('',#23117,#4585);
#3275=LINE('',#23120,#4586);
#3276=LINE('',#23122,#4587);
#3277=LINE('',#23124,#4588);
#3278=LINE('',#23125,#4589);
#3279=LINE('',#23128,#4590);
#3280=LINE('',#23418,#4591);
#3281=LINE('',#23597,#4592);
#3282=LINE('',#23620,#4593);
#3283=LINE('',#23628,#4594);
#3284=LINE('',#23632,#4595);
#3285=LINE('',#23680,#4596);
#3286=LINE('',#23711,#4597);
#3287=LINE('',#23713,#4598);
#3288=LINE('',#23715,#4599);
#3289=LINE('',#23717,#4600);
#3290=LINE('',#23718,#4601);
#3291=LINE('',#23721,#4602);
#3292=LINE('',#23732,#4603);
#3293=LINE('',#23734,#4604);
#3294=LINE('',#23843,#4605);
#3295=LINE('',#23984,#4606);
#3296=LINE('',#23991,#4607);
#3297=LINE('',#23994,#4608);
#3298=LINE('',#24036,#4609);
#3299=LINE('',#24059,#4610);
#3300=LINE('',#24148,#4611);
#3301=LINE('',#24150,#4612);
#3302=LINE('',#24152,#4613);
#3303=LINE('',#24153,#4614);
#3304=LINE('',#24428,#4615);
#3305=LINE('',#24432,#4616);
#3306=LINE('',#24436,#4617);
#3307=LINE('',#24484,#4618);
#3308=LINE('',#24515,#4619);
#3309=LINE('',#24519,#4620);
#3310=LINE('',#24522,#4621);
#3311=LINE('',#24541,#4622);
#3312=LINE('',#24556,#4623);
#3313=LINE('',#24559,#4624);
#3314=LINE('',#24573,#4625);
#3315=LINE('',#24701,#4626);
#3316=LINE('',#24826,#4627);
#3317=LINE('',#24859,#4628);
#3318=LINE('',#24868,#4629);
#3319=LINE('',#24870,#4630);
#3320=LINE('',#24871,#4631);
#3321=LINE('',#24916,#4632);
#3322=LINE('',#24918,#4633);
#3323=LINE('',#24920,#4634);
#3324=LINE('',#24922,#4635);
#3325=LINE('',#24924,#4636);
#3326=LINE('',#24926,#4637);
#3327=LINE('',#24927,#4638);
#3328=LINE('',#24930,#4639);
#3329=LINE('',#24986,#4640);
#3330=LINE('',#24987,#4641);
#3331=LINE('',#24990,#4642);
#3332=LINE('',#25120,#4643);
#3333=LINE('',#25221,#4644);
#3334=LINE('',#25230,#4645);
#3335=LINE('',#25231,#4646);
#3336=LINE('',#25508,#4647);
#3337=LINE('',#25541,#4648);
#3338=LINE('',#25550,#4649);
#3339=LINE('',#25552,#4650);
#3340=LINE('',#25553,#4651);
#3341=LINE('',#25592,#4652);
#3342=LINE('',#25648,#4653);
#3343=LINE('',#25649,#4654);
#3344=LINE('',#25652,#4655);
#3345=LINE('',#25708,#4656);
#3346=LINE('',#25709,#4657);
#3347=LINE('',#25710,#4658);
#3348=LINE('',#25892,#4659);
#3349=LINE('',#25895,#4660);
#3350=LINE('',#25896,#4661);
#3351=LINE('',#25928,#4662);
#3352=LINE('',#25930,#4663);
#3353=LINE('',#25933,#4664);
#3354=LINE('',#25935,#4665);
#3355=LINE('',#25947,#4666);
#3356=LINE('',#25951,#4667);
#3357=LINE('',#25953,#4668);
#3358=LINE('',#25954,#4669);
#3359=LINE('',#25965,#4670);
#3360=LINE('',#25967,#4671);
#3361=LINE('',#25971,#4672);
#3362=LINE('',#25977,#4673);
#3363=LINE('',#25978,#4674);
#3364=LINE('',#25983,#4675);
#3365=LINE('',#25989,#4676);
#3366=LINE('',#25995,#4677);
#3367=LINE('',#26002,#4678);
#3368=LINE('',#26006,#4679);
#3369=LINE('',#26010,#4680);
#3370=LINE('',#26013,#4681);
#3371=LINE('',#26016,#4682);
#3372=LINE('',#26027,#4683);
#3373=LINE('',#26031,#4684);
#3374=LINE('',#26033,#4685);
#3375=LINE('',#26034,#4686);
#3376=LINE('',#26045,#4687);
#3377=LINE('',#26047,#4688);
#3378=LINE('',#26051,#4689);
#3379=LINE('',#26057,#4690);
#3380=LINE('',#26058,#4691);
#3381=LINE('',#26063,#4692);
#3382=LINE('',#26069,#4693);
#3383=LINE('',#26073,#4694);
#3384=LINE('',#26075,#4695);
#3385=LINE('',#26076,#4696);
#3386=LINE('',#26080,#4697);
#3387=LINE('',#26086,#4698);
#3388=LINE('',#26087,#4699);
#3389=LINE('',#26088,#4700);
#3390=LINE('',#26092,#4701);
#3391=LINE('',#26096,#4702);
#3392=LINE('',#26097,#4703);
#3393=LINE('',#26100,#4704);
#3394=LINE('',#26102,#4705);
#3395=LINE('',#26104,#4706);
#3396=LINE('',#26106,#4707);
#3397=LINE('',#26108,#4708);
#3398=LINE('',#26110,#4709);
#3399=LINE('',#26112,#4710);
#3400=LINE('',#26113,#4711);
#3401=LINE('',#26114,#4712);
#3402=LINE('',#26117,#4713);
#3403=LINE('',#26121,#4714);
#3404=LINE('',#26122,#4715);
#3405=LINE('',#26125,#4716);
#3406=LINE('',#26128,#4717);
#3407=LINE('',#26130,#4718);
#3408=LINE('',#26132,#4719);
#3409=LINE('',#26134,#4720);
#3410=LINE('',#26136,#4721);
#3411=LINE('',#26138,#4722);
#3412=LINE('',#26140,#4723);
#3413=LINE('',#26141,#4724);
#3414=LINE('',#26144,#4725);
#3415=LINE('',#26145,#4726);
#3416=LINE('',#26149,#4727);
#3417=LINE('',#26155,#4728);
#3418=LINE('',#26156,#4729);
#3419=LINE('',#26157,#4730);
#3420=LINE('',#26160,#4731);
#3421=LINE('',#26164,#4732);
#3422=LINE('',#26167,#4733);
#3423=LINE('',#26171,#4734);
#3424=LINE('',#26172,#4735);
#3425=LINE('',#26176,#4736);
#3426=LINE('',#26178,#4737);
#3427=LINE('',#26181,#4738);
#3428=LINE('',#26183,#4739);
#3429=LINE('',#26185,#4740);
#3430=LINE('',#26187,#4741);
#3431=LINE('',#26189,#4742);
#3432=LINE('',#26192,#4743);
#3433=LINE('',#26195,#4744);
#3434=LINE('',#26198,#4745);
#3435=LINE('',#26202,#4746);
#3436=LINE('',#26204,#4747);
#3437=LINE('',#26205,#4748);
#3438=LINE('',#26208,#4749);
#3439=LINE('',#26210,#4750);
#3440=LINE('',#26211,#4751);
#3441=LINE('',#26213,#4752);
#3442=LINE('',#26214,#4753);
#3443=LINE('',#26217,#4754);
#3444=LINE('',#26220,#4755);
#3445=LINE('',#26223,#4756);
#3446=LINE('',#26224,#4757);
#3447=LINE('',#26227,#4758);
#3448=LINE('',#26231,#4759);
#3449=LINE('',#26232,#4760);
#3450=LINE('',#26233,#4761);
#3451=LINE('',#26236,#4762);
#3452=LINE('',#26240,#4763);
#3453=LINE('',#26241,#4764);
#3454=LINE('',#26244,#4765);
#3455=LINE('',#26247,#4766);
#3456=LINE('',#26248,#4767);
#3457=LINE('',#26250,#4768);
#3458=LINE('',#26254,#4769);
#3459=LINE('',#26256,#4770);
#3460=LINE('',#26258,#4771);
#3461=LINE('',#26259,#4772);
#3462=LINE('',#26262,#4773);
#3463=LINE('',#26264,#4774);
#3464=LINE('',#26266,#4775);
#3465=LINE('',#26267,#4776);
#3466=LINE('',#26270,#4777);
#3467=LINE('',#26272,#4778);
#3468=LINE('',#26274,#4779);
#3469=LINE('',#26275,#4780);
#3470=LINE('',#26278,#4781);
#3471=LINE('',#26280,#4782);
#3472=LINE('',#26282,#4783);
#3473=LINE('',#26283,#4784);
#3474=LINE('',#26286,#4785);
#3475=LINE('',#26287,#4786);
#3476=LINE('',#26291,#4787);
#3477=LINE('',#26296,#4788);
#3478=LINE('',#26297,#4789);
#3479=LINE('',#26298,#4790);
#3480=LINE('',#26301,#4791);
#3481=LINE('',#26304,#4792);
#3482=LINE('',#26308,#4793);
#3483=LINE('',#26309,#4794);
#3484=LINE('',#26312,#4795);
#3485=LINE('',#26316,#4796);
#3486=LINE('',#26317,#4797);
#3487=LINE('',#26320,#4798);
#3488=LINE('',#26323,#4799);
#3489=LINE('',#26327,#4800);
#3490=LINE('',#26329,#4801);
#3491=LINE('',#26330,#4802);
#3492=LINE('',#26333,#4803);
#3493=LINE('',#26335,#4804);
#3494=LINE('',#26336,#4805);
#3495=LINE('',#26338,#4806);
#3496=LINE('',#26340,#4807);
#3497=LINE('',#26343,#4808);
#3498=LINE('',#26345,#4809);
#3499=LINE('',#26346,#4810);
#3500=LINE('',#26349,#4811);
#3501=LINE('',#26350,#4812);
#3502=LINE('',#26355,#4813);
#3503=LINE('',#26357,#4814);
#3504=LINE('',#26358,#4815);
#3505=LINE('',#26361,#4816);
#3506=LINE('',#26363,#4817);
#3507=LINE('',#26364,#4818);
#3508=LINE('',#26366,#4819);
#3509=LINE('',#26368,#4820);
#3510=LINE('',#26371,#4821);
#3511=LINE('',#26373,#4822);
#3512=LINE('',#26374,#4823);
#3513=LINE('',#26377,#4824);
#3514=LINE('',#26378,#4825);
#3515=LINE('',#26383,#4826);
#3516=LINE('',#26385,#4827);
#3517=LINE('',#26386,#4828);
#3518=LINE('',#26389,#4829);
#3519=LINE('',#26391,#4830);
#3520=LINE('',#26392,#4831);
#3521=LINE('',#26394,#4832);
#3522=LINE('',#26396,#4833);
#3523=LINE('',#26399,#4834);
#3524=LINE('',#26401,#4835);
#3525=LINE('',#26402,#4836);
#3526=LINE('',#26405,#4837);
#3527=LINE('',#26406,#4838);
#3528=LINE('',#26411,#4839);
#3529=LINE('',#26413,#4840);
#3530=LINE('',#26414,#4841);
#3531=LINE('',#26417,#4842);
#3532=LINE('',#26419,#4843);
#3533=LINE('',#26420,#4844);
#3534=LINE('',#26422,#4845);
#3535=LINE('',#26424,#4846);
#3536=LINE('',#26427,#4847);
#3537=LINE('',#26429,#4848);
#3538=LINE('',#26430,#4849);
#3539=LINE('',#26433,#4850);
#3540=LINE('',#26434,#4851);
#3541=LINE('',#26439,#4852);
#3542=LINE('',#26443,#4853);
#3543=LINE('',#26447,#4854);
#3544=LINE('',#26451,#4855);
#3545=LINE('',#26454,#4856);
#3546=LINE('',#26457,#4857);
#3547=LINE('',#26458,#4858);
#3548=LINE('',#26460,#4859);
#3549=LINE('',#26464,#4860);
#3550=LINE('',#26465,#4861);
#3551=LINE('',#26467,#4862);
#3552=LINE('',#26471,#4863);
#3553=LINE('',#26472,#4864);
#3554=LINE('',#26474,#4865);
#3555=LINE('',#26478,#4866);
#3556=LINE('',#26479,#4867);
#3557=LINE('',#26481,#4868);
#3558=LINE('',#26484,#4869);
#3559=LINE('',#26490,#4870);
#3560=LINE('',#26498,#4871);
#3561=LINE('',#26504,#4872);
#3562=LINE('',#26511,#4873);
#3563=LINE('',#26517,#4874);
#3564=LINE('',#26523,#4875);
#3565=LINE('',#26531,#4876);
#3566=LINE('',#26535,#4877);
#3567=LINE('',#26539,#4878);
#3568=LINE('',#26545,#4879);
#3569=LINE('',#26547,#4880);
#3570=LINE('',#26549,#4881);
#3571=LINE('',#26550,#4882);
#3572=LINE('',#26553,#4883);
#3573=LINE('',#26555,#4884);
#3574=LINE('',#26556,#4885);
#3575=LINE('',#26559,#4886);
#3576=LINE('',#26561,#4887);
#3577=LINE('',#26562,#4888);
#3578=LINE('',#26565,#4889);
#3579=LINE('',#26567,#4890);
#3580=LINE('',#26568,#4891);
#3581=LINE('',#26571,#4892);
#3582=LINE('',#26573,#4893);
#3583=LINE('',#26574,#4894);
#3584=LINE('',#26577,#4895);
#3585=LINE('',#26579,#4896);
#3586=LINE('',#26580,#4897);
#3587=LINE('',#26583,#4898);
#3588=LINE('',#26585,#4899);
#3589=LINE('',#26586,#4900);
#3590=LINE('',#26589,#4901);
#3591=LINE('',#26591,#4902);
#3592=LINE('',#26592,#4903);
#3593=LINE('',#26595,#4904);
#3594=LINE('',#26597,#4905);
#3595=LINE('',#26598,#4906);
#3596=LINE('',#26601,#4907);
#3597=LINE('',#26603,#4908);
#3598=LINE('',#26604,#4909);
#3599=LINE('',#26607,#4910);
#3600=LINE('',#26609,#4911);
#3601=LINE('',#26610,#4912);
#3602=LINE('',#26613,#4913);
#3603=LINE('',#26615,#4914);
#3604=LINE('',#26616,#4915);
#3605=LINE('',#26619,#4916);
#3606=LINE('',#26621,#4917);
#3607=LINE('',#26622,#4918);
#3608=LINE('',#26625,#4919);
#3609=LINE('',#26627,#4920);
#3610=LINE('',#26628,#4921);
#3611=LINE('',#26631,#4922);
#3612=LINE('',#26633,#4923);
#3613=LINE('',#26634,#4924);
#3614=LINE('',#26637,#4925);
#3615=LINE('',#26639,#4926);
#3616=LINE('',#26640,#4927);
#3617=LINE('',#26643,#4928);
#3618=LINE('',#26645,#4929);
#3619=LINE('',#26646,#4930);
#3620=LINE('',#26649,#4931);
#3621=LINE('',#26651,#4932);
#3622=LINE('',#26652,#4933);
#3623=LINE('',#26655,#4934);
#3624=LINE('',#26657,#4935);
#3625=LINE('',#26658,#4936);
#3626=LINE('',#26661,#4937);
#3627=LINE('',#26663,#4938);
#3628=LINE('',#26664,#4939);
#3629=LINE('',#26667,#4940);
#3630=LINE('',#26669,#4941);
#3631=LINE('',#26670,#4942);
#3632=LINE('',#26673,#4943);
#3633=LINE('',#26675,#4944);
#3634=LINE('',#26676,#4945);
#3635=LINE('',#26679,#4946);
#3636=LINE('',#26681,#4947);
#3637=LINE('',#26682,#4948);
#3638=LINE('',#26685,#4949);
#3639=LINE('',#26687,#4950);
#3640=LINE('',#26688,#4951);
#3641=LINE('',#26691,#4952);
#3642=LINE('',#26693,#4953);
#3643=LINE('',#26694,#4954);
#3644=LINE('',#26697,#4955);
#3645=LINE('',#26699,#4956);
#3646=LINE('',#26700,#4957);
#3647=LINE('',#26703,#4958);
#3648=LINE('',#26705,#4959);
#3649=LINE('',#26706,#4960);
#3650=LINE('',#26709,#4961);
#3651=LINE('',#26711,#4962);
#3652=LINE('',#26712,#4963);
#3653=LINE('',#26715,#4964);
#3654=LINE('',#26717,#4965);
#3655=LINE('',#26718,#4966);
#3656=LINE('',#26721,#4967);
#3657=LINE('',#26723,#4968);
#3658=LINE('',#26724,#4969);
#3659=LINE('',#26727,#4970);
#3660=LINE('',#26729,#4971);
#3661=LINE('',#26730,#4972);
#3662=LINE('',#26733,#4973);
#3663=LINE('',#26735,#4974);
#3664=LINE('',#26736,#4975);
#3665=LINE('',#26739,#4976);
#3666=LINE('',#26741,#4977);
#3667=LINE('',#26742,#4978);
#3668=LINE('',#26745,#4979);
#3669=LINE('',#26747,#4980);
#3670=LINE('',#26748,#4981);
#3671=LINE('',#26751,#4982);
#3672=LINE('',#26753,#4983);
#3673=LINE('',#26754,#4984);
#3674=LINE('',#26757,#4985);
#3675=LINE('',#26759,#4986);
#3676=LINE('',#26760,#4987);
#3677=LINE('',#26763,#4988);
#3678=LINE('',#26765,#4989);
#3679=LINE('',#26766,#4990);
#3680=LINE('',#26769,#4991);
#3681=LINE('',#26771,#4992);
#3682=LINE('',#26772,#4993);
#3683=LINE('',#26775,#4994);
#3684=LINE('',#26777,#4995);
#3685=LINE('',#26778,#4996);
#3686=LINE('',#26781,#4997);
#3687=LINE('',#26783,#4998);
#3688=LINE('',#26784,#4999);
#3689=LINE('',#26787,#5000);
#3690=LINE('',#26789,#5001);
#3691=LINE('',#26790,#5002);
#3692=LINE('',#26793,#5003);
#3693=LINE('',#26795,#5004);
#3694=LINE('',#26796,#5005);
#3695=LINE('',#26799,#5006);
#3696=LINE('',#26801,#5007);
#3697=LINE('',#26802,#5008);
#3698=LINE('',#26805,#5009);
#3699=LINE('',#26807,#5010);
#3700=LINE('',#26808,#5011);
#3701=LINE('',#26811,#5012);
#3702=LINE('',#26813,#5013);
#3703=LINE('',#26814,#5014);
#3704=LINE('',#26817,#5015);
#3705=LINE('',#26819,#5016);
#3706=LINE('',#26820,#5017);
#3707=LINE('',#26823,#5018);
#3708=LINE('',#26825,#5019);
#3709=LINE('',#26826,#5020);
#3710=LINE('',#26829,#5021);
#3711=LINE('',#26831,#5022);
#3712=LINE('',#26832,#5023);
#3713=LINE('',#26835,#5024);
#3714=LINE('',#26837,#5025);
#3715=LINE('',#26838,#5026);
#3716=LINE('',#26840,#5027);
#3717=LINE('',#26841,#5028);
#3718=LINE('',#26848,#5029);
#3719=LINE('',#26850,#5030);
#3720=LINE('',#26852,#5031);
#3721=LINE('',#26853,#5032);
#3722=LINE('',#26857,#5033);
#3723=LINE('',#26863,#5034);
#3724=LINE('',#26864,#5035);
#3725=LINE('',#26865,#5036);
#3726=LINE('',#26869,#5037);
#3727=LINE('',#26875,#5038);
#3728=LINE('',#26876,#5039);
#3729=LINE('',#26877,#5040);
#3730=LINE('',#26881,#5041);
#3731=LINE('',#26887,#5042);
#3732=LINE('',#26888,#5043);
#3733=LINE('',#26889,#5044);
#3734=LINE('',#26895,#5045);
#3735=LINE('',#26898,#5046);
#3736=LINE('',#26901,#5047);
#3737=LINE('',#26902,#5048);
#3738=LINE('',#26905,#5049);
#3739=LINE('',#26909,#5050);
#3740=LINE('',#26910,#5051);
#3741=LINE('',#26914,#5052);
#3742=LINE('',#26918,#5053);
#3743=LINE('',#26922,#5054);
#3744=LINE('',#26926,#5055);
#3745=LINE('',#26931,#5056);
#3746=LINE('',#26935,#5057);
#3747=LINE('',#26940,#5058);
#3748=LINE('',#26941,#5059);
#3749=LINE('',#26942,#5060);
#3750=LINE('',#26946,#5061);
#3751=LINE('',#26952,#5062);
#3752=LINE('',#26953,#5063);
#3753=LINE('',#26954,#5064);
#3754=LINE('',#26958,#5065);
#3755=LINE('',#26964,#5066);
#3756=LINE('',#26965,#5067);
#3757=LINE('',#26966,#5068);
#3758=LINE('',#26970,#5069);
#3759=LINE('',#26974,#5070);
#3760=LINE('',#26975,#5071);
#3761=LINE('',#26977,#5072);
#3762=LINE('',#26978,#5073);
#3763=LINE('',#26980,#5074);
#3764=LINE('',#26982,#5075);
#3765=LINE('',#26984,#5076);
#3766=LINE('',#26990,#5077);
#3767=LINE('',#26994,#5078);
#3768=LINE('',#26998,#5079);
#3769=LINE('',#27001,#5080);
#3770=LINE('',#27004,#5081);
#3771=LINE('',#27006,#5082);
#3772=LINE('',#27010,#5083);
#3773=LINE('',#27011,#5084);
#3774=LINE('',#27014,#5085);
#3775=LINE('',#27018,#5086);
#3776=LINE('',#27019,#5087);
#3777=LINE('',#27022,#5088);
#3778=LINE('',#27026,#5089);
#3779=LINE('',#27027,#5090);
#3780=LINE('',#27030,#5091);
#3781=LINE('',#27033,#5092);
#3782=LINE('',#27036,#5093);
#3783=LINE('',#27038,#5094);
#3784=LINE('',#27040,#5095);
#3785=LINE('',#27042,#5096);
#3786=LINE('',#27043,#5097);
#3787=LINE('',#27046,#5098);
#3788=LINE('',#27210,#5099);
#3789=LINE('',#27212,#5100);
#3790=LINE('',#27214,#5101);
#3791=LINE('',#27215,#5102);
#3792=LINE('',#27218,#5103);
#3793=LINE('',#27801,#5104);
#3794=LINE('',#27829,#5105);
#3795=LINE('',#27838,#5106);
#3796=LINE('',#27842,#5107);
#3797=LINE('',#27910,#5108);
#3798=LINE('',#28050,#5109);
#3799=LINE('',#28052,#5110);
#3800=LINE('',#28265,#5111);
#3801=LINE('',#28478,#5112);
#3802=LINE('',#28521,#5113);
#3803=LINE('',#28533,#5114);
#3804=LINE('',#28537,#5115);
#3805=LINE('',#28590,#5116);
#3806=LINE('',#28621,#5117);
#3807=LINE('',#28622,#5118);
#3808=LINE('',#28624,#5119);
#3809=LINE('',#28626,#5120);
#3810=LINE('',#28629,#5121);
#3811=LINE('',#28632,#5122);
#3812=LINE('',#28635,#5123);
#3813=LINE('',#28636,#5124);
#3814=LINE('',#28639,#5125);
#3815=LINE('',#28643,#5126);
#3816=LINE('',#28644,#5127);
#3817=LINE('',#28648,#5128);
#3818=LINE('',#28654,#5129);
#3819=LINE('',#28655,#5130);
#3820=LINE('',#28656,#5131);
#3821=LINE('',#28660,#5132);
#3822=LINE('',#28664,#5133);
#3823=LINE('',#28665,#5134);
#3824=LINE('',#28680,#5135);
#3825=LINE('',#28693,#5136);
#3826=LINE('',#28908,#5137);
#3827=LINE('',#28910,#5138);
#3828=LINE('',#28911,#5139);
#3829=LINE('',#28953,#5140);
#3830=LINE('',#29217,#5141);
#3831=LINE('',#29282,#5142);
#3832=LINE('',#29284,#5143);
#3833=LINE('',#29285,#5144);
#3834=LINE('',#29332,#5145);
#3835=LINE('',#29350,#5146);
#3836=LINE('',#29353,#5147);
#3837=LINE('',#29355,#5148);
#3838=LINE('',#29357,#5149);
#3839=LINE('',#29360,#5150);
#3840=LINE('',#29361,#5151);
#3841=LINE('',#29363,#5152);
#3842=LINE('',#29370,#5153);
#3843=LINE('',#29372,#5154);
#3844=LINE('',#29374,#5155);
#3845=LINE('',#29376,#5156);
#3846=LINE('',#29378,#5157);
#3847=LINE('',#29379,#5158);
#3848=LINE('',#29383,#5159);
#3849=LINE('',#29389,#5160);
#3850=LINE('',#29390,#5161);
#3851=LINE('',#29391,#5162);
#3852=LINE('',#29395,#5163);
#3853=LINE('',#29401,#5164);
#3854=LINE('',#29402,#5165);
#3855=LINE('',#29403,#5166);
#3856=LINE('',#29407,#5167);
#3857=LINE('',#29413,#5168);
#3858=LINE('',#29414,#5169);
#3859=LINE('',#29415,#5170);
#3860=LINE('',#29421,#5171);
#3861=LINE('',#29423,#5172);
#3862=LINE('',#29425,#5173);
#3863=LINE('',#29429,#5174);
#3864=LINE('',#29433,#5175);
#3865=LINE('',#29437,#5176);
#3866=LINE('',#29441,#5177);
#3867=LINE('',#29443,#5178);
#3868=LINE('',#29444,#5179);
#3869=LINE('',#29447,#5180);
#3870=LINE('',#29450,#5181);
#3871=LINE('',#29453,#5182);
#3872=LINE('',#29454,#5183);
#3873=LINE('',#29457,#5184);
#3874=LINE('',#29461,#5185);
#3875=LINE('',#29462,#5186);
#3876=LINE('',#29466,#5187);
#3877=LINE('',#29468,#5188);
#3878=LINE('',#29469,#5189);
#3879=LINE('',#29473,#5190);
#3880=LINE('',#29474,#5191);
#3881=LINE('',#29476,#5192);
#3882=LINE('',#29477,#5193);
#3883=LINE('',#29481,#5194);
#3884=LINE('',#29482,#5195);
#3885=LINE('',#29484,#5196);
#3886=LINE('',#29485,#5197);
#3887=LINE('',#29487,#5198);
#3888=LINE('',#29488,#5199);
#3889=LINE('',#29491,#5200);
#3890=LINE('',#29492,#5201);
#3891=LINE('',#29495,#5202);
#3892=LINE('',#29497,#5203);
#3893=LINE('',#29498,#5204);
#3894=LINE('',#29500,#5205);
#3895=LINE('',#29501,#5206);
#3896=LINE('',#29707,#5207);
#3897=LINE('',#29912,#5208);
#3898=LINE('',#29940,#5209);
#3899=LINE('',#29949,#5210);
#3900=LINE('',#29953,#5211);
#3901=LINE('',#30006,#5212);
#3902=LINE('',#30038,#5213);
#3903=LINE('',#30140,#5214);
#3904=LINE('',#30143,#5215);
#3905=LINE('',#30145,#5216);
#3906=LINE('',#30147,#5217);
#3907=LINE('',#30148,#5218);
#3908=LINE('',#30151,#5219);
#3909=LINE('',#30365,#5220);
#3910=LINE('',#30499,#5221);
#3911=LINE('',#30503,#5222);
#3912=LINE('',#30507,#5223);
#3913=LINE('',#30560,#5224);
#3914=LINE('',#30592,#5225);
#3915=LINE('',#30606,#5226);
#3916=LINE('',#30619,#5227);
#3917=LINE('',#30622,#5228);
#3918=LINE('',#30623,#5229);
#3919=LINE('',#30626,#5230);
#3920=LINE('',#30627,#5231);
#3921=LINE('',#30631,#5232);
#3922=LINE('',#30632,#5233);
#3923=LINE('',#30633,#5234);
#3924=LINE('',#30636,#5235);
#3925=LINE('',#30640,#5236);
#3926=LINE('',#30641,#5237);
#3927=LINE('',#30643,#5238);
#3928=LINE('',#30646,#5239);
#3929=LINE('',#30648,#5240);
#3930=LINE('',#30651,#5241);
#3931=LINE('',#30652,#5242);
#3932=LINE('',#30655,#5243);
#3933=LINE('',#30659,#5244);
#3934=LINE('',#30660,#5245);
#3935=LINE('',#30662,#5246);
#3936=LINE('',#30663,#5247);
#3937=LINE('',#30665,#5248);
#3938=LINE('',#30666,#5249);
#3939=LINE('',#30668,#5250);
#3940=LINE('',#30671,#5251);
#3941=LINE('',#30673,#5252);
#3942=LINE('',#30674,#5253);
#3943=LINE('',#30677,#5254);
#3944=LINE('',#31064,#5255);
#3945=LINE('',#31269,#5256);
#3946=LINE('',#31296,#5257);
#3947=LINE('',#31304,#5258);
#3948=LINE('',#31307,#5259);
#3949=LINE('',#31354,#5260);
#3950=LINE('',#31381,#5261);
#3951=LINE('',#31383,#5262);
#3952=LINE('',#31385,#5263);
#3953=LINE('',#31526,#5264);
#3954=LINE('',#31678,#5265);
#3955=LINE('',#31685,#5266);
#3956=LINE('',#31686,#5267);
#3957=LINE('',#31728,#5268);
#3958=LINE('',#31747,#5269);
#3959=LINE('',#31751,#5270);
#3960=LINE('',#31755,#5271);
#3961=LINE('',#31756,#5272);
#3962=LINE('',#31759,#5273);
#3963=LINE('',#31762,#5274);
#3964=LINE('',#31769,#5275);
#3965=LINE('',#31774,#5276);
#3966=LINE('',#31778,#5277);
#3967=LINE('',#31780,#5278);
#3968=LINE('',#31782,#5279);
#3969=LINE('',#31784,#5280);
#3970=LINE('',#31786,#5281);
#3971=LINE('',#31788,#5282);
#3972=LINE('',#31790,#5283);
#3973=LINE('',#31792,#5284);
#3974=LINE('',#31794,#5285);
#3975=LINE('',#31795,#5286);
#3976=LINE('',#31799,#5287);
#3977=LINE('',#31803,#5288);
#3978=LINE('',#31805,#5289);
#3979=LINE('',#31807,#5290);
#3980=LINE('',#31809,#5291);
#3981=LINE('',#31811,#5292);
#3982=LINE('',#31813,#5293);
#3983=LINE('',#31815,#5294);
#3984=LINE('',#31817,#5295);
#3985=LINE('',#31819,#5296);
#3986=LINE('',#31821,#5297);
#3987=LINE('',#31823,#5298);
#3988=LINE('',#31825,#5299);
#3989=LINE('',#31827,#5300);
#3990=LINE('',#31829,#5301);
#3991=LINE('',#31831,#5302);
#3992=LINE('',#31833,#5303);
#3993=LINE('',#31835,#5304);
#3994=LINE('',#31837,#5305);
#3995=LINE('',#31839,#5306);
#3996=LINE('',#31841,#5307);
#3997=LINE('',#31843,#5308);
#3998=LINE('',#31845,#5309);
#3999=LINE('',#31847,#5310);
#4000=LINE('',#31849,#5311);
#4001=LINE('',#31851,#5312);
#4002=LINE('',#31853,#5313);
#4003=LINE('',#31855,#5314);
#4004=LINE('',#31857,#5315);
#4005=LINE('',#31859,#5316);
#4006=LINE('',#31861,#5317);
#4007=LINE('',#31863,#5318);
#4008=LINE('',#31865,#5319);
#4009=LINE('',#31867,#5320);
#4010=LINE('',#31869,#5321);
#4011=LINE('',#31871,#5322);
#4012=LINE('',#31873,#5323);
#4013=LINE('',#31875,#5324);
#4014=LINE('',#31877,#5325);
#4015=LINE('',#31879,#5326);
#4016=LINE('',#31881,#5327);
#4017=LINE('',#31883,#5328);
#4018=LINE('',#31885,#5329);
#4019=LINE('',#31887,#5330);
#4020=LINE('',#31889,#5331);
#4021=LINE('',#31891,#5332);
#4022=LINE('',#31893,#5333);
#4023=LINE('',#31895,#5334);
#4024=LINE('',#31897,#5335);
#4025=LINE('',#31899,#5336);
#4026=LINE('',#31901,#5337);
#4027=LINE('',#31903,#5338);
#4028=LINE('',#31905,#5339);
#4029=LINE('',#31907,#5340);
#4030=LINE('',#31909,#5341);
#4031=LINE('',#31911,#5342);
#4032=LINE('',#31913,#5343);
#4033=LINE('',#31915,#5344);
#4034=LINE('',#31917,#5345);
#4035=LINE('',#31919,#5346);
#4036=LINE('',#31920,#5347);
#4037=LINE('',#31923,#5348);
#4038=LINE('',#31925,#5349);
#4039=LINE('',#31926,#5350);
#4040=LINE('',#31929,#5351);
#4041=LINE('',#31931,#5352);
#4042=LINE('',#31932,#5353);
#4043=LINE('',#31935,#5354);
#4044=LINE('',#31937,#5355);
#4045=LINE('',#31938,#5356);
#4046=LINE('',#31941,#5357);
#4047=LINE('',#31943,#5358);
#4048=LINE('',#31944,#5359);
#4049=LINE('',#31947,#5360);
#4050=LINE('',#31949,#5361);
#4051=LINE('',#31950,#5362);
#4052=LINE('',#31953,#5363);
#4053=LINE('',#31955,#5364);
#4054=LINE('',#31956,#5365);
#4055=LINE('',#31960,#5366);
#4056=LINE('',#31961,#5367);
#4057=LINE('',#31962,#5368);
#4058=LINE('',#31965,#5369);
#4059=LINE('',#31967,#5370);
#4060=LINE('',#31968,#5371);
#4061=LINE('',#31972,#5372);
#4062=LINE('',#31973,#5373);
#4063=LINE('',#31974,#5374);
#4064=LINE('',#31976,#5375);
#4065=LINE('',#31980,#5376);
#4066=LINE('',#31981,#5377);
#4067=LINE('',#31982,#5378);
#4068=LINE('',#31984,#5379);
#4069=LINE('',#31988,#5380);
#4070=LINE('',#31989,#5381);
#4071=LINE('',#31990,#5382);
#4072=LINE('',#31992,#5383);
#4073=LINE('',#31993,#5384);
#4074=LINE('',#31995,#5385);
#4075=LINE('',#31996,#5386);
#4076=LINE('',#31998,#5387);
#4077=LINE('',#31999,#5388);
#4078=LINE('',#32002,#5389);
#4079=LINE('',#32004,#5390);
#4080=LINE('',#32005,#5391);
#4081=LINE('',#32008,#5392);
#4082=LINE('',#32010,#5393);
#4083=LINE('',#32011,#5394);
#4084=LINE('',#32013,#5395);
#4085=LINE('',#32015,#5396);
#4086=LINE('',#32017,#5397);
#4087=LINE('',#32018,#5398);
#4088=LINE('',#32021,#5399);
#4089=LINE('',#32022,#5400);
#4090=LINE('',#32025,#5401);
#4091=LINE('',#32026,#5402);
#4092=LINE('',#32029,#5403);
#4093=LINE('',#32031,#5404);
#4094=LINE('',#32032,#5405);
#4095=LINE('',#32035,#5406);
#4096=LINE('',#32037,#5407);
#4097=LINE('',#32038,#5408);
#4098=LINE('',#32041,#5409);
#4099=LINE('',#32043,#5410);
#4100=LINE('',#32044,#5411);
#4101=LINE('',#32047,#5412);
#4102=LINE('',#32049,#5413);
#4103=LINE('',#32050,#5414);
#4104=LINE('',#32053,#5415);
#4105=LINE('',#32055,#5416);
#4106=LINE('',#32056,#5417);
#4107=LINE('',#32059,#5418);
#4108=LINE('',#32061,#5419);
#4109=LINE('',#32062,#5420);
#4110=LINE('',#32065,#5421);
#4111=LINE('',#32067,#5422);
#4112=LINE('',#32068,#5423);
#4113=LINE('',#32071,#5424);
#4114=LINE('',#32073,#5425);
#4115=LINE('',#32074,#5426);
#4116=LINE('',#32077,#5427);
#4117=LINE('',#32079,#5428);
#4118=LINE('',#32080,#5429);
#4119=LINE('',#32083,#5430);
#4120=LINE('',#32085,#5431);
#4121=LINE('',#32086,#5432);
#4122=LINE('',#32089,#5433);
#4123=LINE('',#32091,#5434);
#4124=LINE('',#32092,#5435);
#4125=LINE('',#32095,#5436);
#4126=LINE('',#32097,#5437);
#4127=LINE('',#32098,#5438);
#4128=LINE('',#32101,#5439);
#4129=LINE('',#32102,#5440);
#4130=LINE('',#32106,#5441);
#4131=LINE('',#32107,#5442);
#4132=LINE('',#32108,#5443);
#4133=LINE('',#32110,#5444);
#4134=LINE('',#32114,#5445);
#4135=LINE('',#32115,#5446);
#4136=LINE('',#32116,#5447);
#4137=LINE('',#32118,#5448);
#4138=LINE('',#32122,#5449);
#4139=LINE('',#32123,#5450);
#4140=LINE('',#32124,#5451);
#4141=LINE('',#32126,#5452);
#4142=LINE('',#32129,#5453);
#4143=LINE('',#32131,#5454);
#4144=LINE('',#32132,#5455);
#4145=LINE('',#32135,#5456);
#4146=LINE('',#32136,#5457);
#4147=LINE('',#32138,#5458);
#4148=LINE('',#32139,#5459);
#4149=LINE('',#32141,#5460);
#4150=LINE('',#32143,#5461);
#4151=LINE('',#32144,#5462);
#4152=LINE('',#32146,#5463);
#4153=LINE('',#32147,#5464);
#4154=LINE('',#32149,#5465);
#4155=LINE('',#32150,#5466);
#4156=LINE('',#32152,#5467);
#4157=LINE('',#32153,#5468);
#4158=LINE('',#32155,#5469);
#4159=LINE('',#32156,#5470);
#4160=LINE('',#32159,#5471);
#4161=LINE('',#32161,#5472);
#4162=LINE('',#32162,#5473);
#4163=LINE('',#32165,#5474);
#4164=LINE('',#32167,#5475);
#4165=LINE('',#32168,#5476);
#4166=LINE('',#32171,#5477);
#4167=LINE('',#32173,#5478);
#4168=LINE('',#32174,#5479);
#4169=LINE('',#32177,#5480);
#4170=LINE('',#32179,#5481);
#4171=LINE('',#32180,#5482);
#4172=LINE('',#32183,#5483);
#4173=LINE('',#32185,#5484);
#4174=LINE('',#32186,#5485);
#4175=LINE('',#32189,#5486);
#4176=LINE('',#32191,#5487);
#4177=LINE('',#32192,#5488);
#4178=LINE('',#32195,#5489);
#4179=LINE('',#32197,#5490);
#4180=LINE('',#32198,#5491);
#4181=LINE('',#32202,#5492);
#4182=LINE('',#32203,#5493);
#4183=LINE('',#32204,#5494);
#4184=LINE('',#32206,#5495);
#4185=LINE('',#32208,#5496);
#4186=LINE('',#32211,#5497);
#4187=LINE('',#32212,#5498);
#4188=LINE('',#32216,#5499);
#4189=LINE('',#32217,#5500);
#4190=LINE('',#32221,#5501);
#4191=LINE('',#32222,#5502);
#4192=LINE('',#32226,#5503);
#4193=LINE('',#32227,#5504);
#4194=LINE('',#32231,#5505);
#4195=LINE('',#32232,#5506);
#4196=LINE('',#32236,#5507);
#4197=LINE('',#32237,#5508);
#4198=LINE('',#32241,#5509);
#4199=LINE('',#32242,#5510);
#4200=LINE('',#32246,#5511);
#4201=LINE('',#32247,#5512);
#4202=LINE('',#32252,#5513);
#4203=LINE('',#32253,#5514);
#4204=LINE('',#32256,#5515);
#4205=LINE('',#32257,#5516);
#4206=LINE('',#32259,#5517);
#4207=VECTOR('',#15010,10.);
#4208=VECTOR('',#15011,10.);
#4209=VECTOR('',#15012,10.);
#4210=VECTOR('',#15013,10.);
#4211=VECTOR('',#15016,10.);
#4212=VECTOR('',#15023,10.);
#4213=VECTOR('',#15024,10.);
#4214=VECTOR('',#15025,10.);
#4215=VECTOR('',#15028,10.);
#4216=VECTOR('',#15035,10.);
#4217=VECTOR('',#15036,10.);
#4218=VECTOR('',#15037,10.);
#4219=VECTOR('',#15040,10.);
#4220=VECTOR('',#15047,10.);
#4221=VECTOR('',#15048,10.);
#4222=VECTOR('',#15049,10.);
#4223=VECTOR('',#15058,10.);
#4224=VECTOR('',#15061,10.);
#4225=VECTOR('',#15064,10.);
#4226=VECTOR('',#15065,10.);
#4227=VECTOR('',#15070,10.);
#4228=VECTOR('',#15075,10.);
#4229=VECTOR('',#15076,10.);
#4230=VECTOR('',#15079,10.);
#4231=VECTOR('',#15082,10.);
#4232=VECTOR('',#15085,10.);
#4233=VECTOR('',#15088,10.);
#4234=VECTOR('',#15093,10.);
#4235=VECTOR('',#15094,10.);
#4236=VECTOR('',#15095,10.);
#4237=VECTOR('',#15098,10.);
#4238=VECTOR('',#15103,10.);
#4239=VECTOR('',#15104,10.);
#4240=VECTOR('',#15107,10.);
#4241=VECTOR('',#15112,10.);
#4242=VECTOR('',#15113,10.);
#4243=VECTOR('',#15116,10.);
#4244=VECTOR('',#15121,10.);
#4245=VECTOR('',#15122,10.);
#4246=VECTOR('',#15129,10.);
#4247=VECTOR('',#15132,10.);
#4248=VECTOR('',#15135,10.);
#4249=VECTOR('',#15136,10.);
#4250=VECTOR('',#15139,10.);
#4251=VECTOR('',#15144,10.);
#4252=VECTOR('',#15145,10.);
#4253=VECTOR('',#15148,10.);
#4254=VECTOR('',#15149,10.);
#4255=VECTOR('',#15150,10.);
#4256=VECTOR('',#15153,10.);
#4257=VECTOR('',#15158,10.);
#4258=VECTOR('',#15159,10.);
#4259=VECTOR('',#15160,10.);
#4260=VECTOR('',#15163,10.);
#4261=VECTOR('',#15170,10.);
#4262=VECTOR('',#15171,10.);
#4263=VECTOR('',#15172,10.);
#4264=VECTOR('',#15175,10.);
#4265=VECTOR('',#15182,10.);
#4266=VECTOR('',#15183,10.);
#4267=VECTOR('',#15190,10.);
#4268=VECTOR('',#15193,10.);
#4269=VECTOR('',#15196,10.);
#4270=VECTOR('',#15199,10.);
#4271=VECTOR('',#15202,10.);
#4272=VECTOR('',#15207,10.);
#4273=VECTOR('',#15208,10.);
#4274=VECTOR('',#15211,10.);
#4275=VECTOR('',#15214,10.);
#4276=VECTOR('',#15215,10.);
#4277=VECTOR('',#15218,10.);
#4278=VECTOR('',#15223,10.);
#4279=VECTOR('',#15224,10.);
#4280=VECTOR('',#15227,10.);
#4281=VECTOR('',#15232,10.);
#4282=VECTOR('',#15237,10.);
#4283=VECTOR('',#15242,5.2);
#4284=VECTOR('',#15245,10.);
#4285=VECTOR('',#15248,10.);
#4286=VECTOR('',#15253,10.);
#4287=VECTOR('',#15256,10.);
#4288=VECTOR('',#15261,10.);
#4289=VECTOR('',#15262,10.);
#4290=VECTOR('',#15263,10.);
#4291=VECTOR('',#15266,10.);
#4292=VECTOR('',#15269,10.);
#4293=VECTOR('',#15272,10.);
#4294=VECTOR('',#15275,10.);
#4295=VECTOR('',#15276,10.);
#4296=VECTOR('',#15279,10.);
#4297=VECTOR('',#15280,10.);
#4298=VECTOR('',#15281,10.);
#4299=VECTOR('',#15282,10.);
#4300=VECTOR('',#15283,10.);
#4301=VECTOR('',#15284,10.);
#4302=VECTOR('',#15287,10.);
#4303=VECTOR('',#15290,10.);
#4304=VECTOR('',#15291,10.);
#4305=VECTOR('',#15294,10.);
#4306=VECTOR('',#15297,10.);
#4307=VECTOR('',#15300,10.);
#4308=VECTOR('',#15303,10.);
#4309=VECTOR('',#15306,10.);
#4310=VECTOR('',#15309,10.);
#4311=VECTOR('',#15310,10.);
#4312=VECTOR('',#15311,10.);
#4313=VECTOR('',#15314,10.);
#4314=VECTOR('',#15317,10.);
#4315=VECTOR('',#15320,10.);
#4316=VECTOR('',#15323,10.);
#4317=VECTOR('',#15326,10.);
#4318=VECTOR('',#15327,10.);
#4319=VECTOR('',#15328,10.);
#4320=VECTOR('',#15331,10.);
#4321=VECTOR('',#15334,10.);
#4322=VECTOR('',#15335,10.);
#4323=VECTOR('',#15338,10.);
#4324=VECTOR('',#15341,10.);
#4325=VECTOR('',#15344,10.);
#4326=VECTOR('',#15347,10.);
#4327=VECTOR('',#15350,10.);
#4328=VECTOR('',#15351,10.);
#4329=VECTOR('',#15354,10.);
#4330=VECTOR('',#15359,10.);
#4331=VECTOR('',#15362,10.);
#4332=VECTOR('',#15363,10.);
#4333=VECTOR('',#15366,10.);
#4334=VECTOR('',#15371,10.);
#4335=VECTOR('',#15374,10.);
#4336=VECTOR('',#15379,10.);
#4337=VECTOR('',#15380,10.);
#4338=VECTOR('',#15381,10.);
#4339=VECTOR('',#15384,10.);
#4340=VECTOR('',#15385,10.);
#4341=VECTOR('',#15386,10.);
#4342=VECTOR('',#15389,10.);
#4343=VECTOR('',#15390,10.);
#4344=VECTOR('',#15393,10.);
#4345=VECTOR('',#15394,10.);
#4346=VECTOR('',#15397,10.);
#4347=VECTOR('',#15400,10.);
#4348=VECTOR('',#15401,10.);
#4349=VECTOR('',#15402,10.);
#4350=VECTOR('',#15403,10.);
#4351=VECTOR('',#15404,10.);
#4352=VECTOR('',#15405,10.);
#4353=VECTOR('',#15406,10.);
#4354=VECTOR('',#15407,10.);
#4355=VECTOR('',#15410,10.);
#4356=VECTOR('',#15411,10.);
#4357=VECTOR('',#15414,10.);
#4358=VECTOR('',#15415,10.);
#4359=VECTOR('',#15418,10.);
#4360=VECTOR('',#15419,10.);
#4361=VECTOR('',#15422,10.);
#4362=VECTOR('',#15423,10.);
#4363=VECTOR('',#15426,10.);
#4364=VECTOR('',#15427,10.);
#4365=VECTOR('',#15428,10.);
#4366=VECTOR('',#15429,10.);
#4367=VECTOR('',#15432,10.);
#4368=VECTOR('',#15433,10.);
#4369=VECTOR('',#15434,10.);
#4370=VECTOR('',#15437,10.);
#4371=VECTOR('',#15440,10.);
#4372=VECTOR('',#15443,10.);
#4373=VECTOR('',#15446,10.);
#4374=VECTOR('',#15447,10.);
#4375=VECTOR('',#15452,10.);
#4376=VECTOR('',#15461,2.7);
#4377=VECTOR('',#15466,2.45);
#4378=VECTOR('',#15471,10.);
#4379=VECTOR('',#15472,10.);
#4380=VECTOR('',#15473,10.);
#4381=VECTOR('',#15474,10.);
#4382=VECTOR('',#15479,2.7);
#4383=VECTOR('',#15482,10.);
#4384=VECTOR('',#15483,10.);
#4385=VECTOR('',#15484,10.);
#4386=VECTOR('',#15485,10.);
#4387=VECTOR('',#15488,10.);
#4388=VECTOR('',#15489,10.);
#4389=VECTOR('',#15490,10.);
#4390=VECTOR('',#15491,10.);
#4391=VECTOR('',#15494,10.);
#4392=VECTOR('',#15501,10.);
#4393=VECTOR('',#15502,10.);
#4394=VECTOR('',#15503,10.);
#4395=VECTOR('',#15506,10.);
#4396=VECTOR('',#15513,10.);
#4397=VECTOR('',#15514,10.);
#4398=VECTOR('',#15517,10.);
#4399=VECTOR('',#15524,10.);
#4400=VECTOR('',#15525,10.);
#4401=VECTOR('',#15526,10.);
#4402=VECTOR('',#15535,10.);
#4403=VECTOR('',#15540,10.);
#4404=VECTOR('',#15541,10.);
#4405=VECTOR('',#15544,10.);
#4406=VECTOR('',#15549,10.);
#4407=VECTOR('',#15550,10.);
#4408=VECTOR('',#15555,10.);
#4409=VECTOR('',#15558,10.);
#4410=VECTOR('',#15561,10.);
#4411=VECTOR('',#15564,10.);
#4412=VECTOR('',#15567,10.);
#4413=VECTOR('',#15568,10.);
#4414=VECTOR('',#15573,10.);
#4415=VECTOR('',#15574,10.);
#4416=VECTOR('',#15577,10.);
#4417=VECTOR('',#15582,10.);
#4418=VECTOR('',#15583,10.);
#4419=VECTOR('',#15586,10.);
#4420=VECTOR('',#15591,10.);
#4421=VECTOR('',#15592,10.);
#4422=VECTOR('',#15595,10.);
#4423=VECTOR('',#15602,10.);
#4424=VECTOR('',#15603,10.);
#4425=VECTOR('',#15604,10.);
#4426=VECTOR('',#15607,10.);
#4427=VECTOR('',#15612,10.);
#4428=VECTOR('',#15613,10.);
#4429=VECTOR('',#15620,10.);
#4430=VECTOR('',#15621,10.);
#4431=VECTOR('',#15622,10.);
#4432=VECTOR('',#15625,10.);
#4433=VECTOR('',#15630,10.);
#4434=VECTOR('',#15631,10.);
#4435=VECTOR('',#15634,10.);
#4436=VECTOR('',#15639,10.);
#4437=VECTOR('',#15640,10.);
#4438=VECTOR('',#15643,10.);
#4439=VECTOR('',#15650,10.);
#4440=VECTOR('',#15651,10.);
#4441=VECTOR('',#15652,10.);
#4442=VECTOR('',#15661,10.);
#4443=VECTOR('',#15664,10.);
#4444=VECTOR('',#15667,10.);
#4445=VECTOR('',#15670,10.);
#4446=VECTOR('',#15675,10.);
#4447=VECTOR('',#15676,10.);
#4448=VECTOR('',#15679,10.);
#4449=VECTOR('',#15682,10.);
#4450=VECTOR('',#15685,10.);
#4451=VECTOR('',#15690,10.);
#4452=VECTOR('',#15691,10.);
#4453=VECTOR('',#15694,10.);
#4454=VECTOR('',#15699,10.);
#4455=VECTOR('',#15704,10.);
#4456=VECTOR('',#15707,10.);
#4457=VECTOR('',#15712,10.);
#4458=VECTOR('',#15715,10.);
#4459=VECTOR('',#15724,5.45);
#4460=VECTOR('',#15729,10.);
#4461=VECTOR('',#15730,10.);
#4462=VECTOR('',#15731,10.);
#4463=VECTOR('',#15732,10.);
#4464=VECTOR('',#15747,5.2);
#4465=VECTOR('',#15750,5.45);
#4466=VECTOR('',#15757,5.2);
#4467=VECTOR('',#15760,5.45);
#4468=VECTOR('',#15767,5.2);
#4469=VECTOR('',#15770,5.45);
#4470=VECTOR('',#15777,5.2);
#4471=VECTOR('',#15780,5.45);
#4472=VECTOR('',#15787,5.2);
#4473=VECTOR('',#15790,5.45);
#4474=VECTOR('',#15797,5.2);
#4475=VECTOR('',#15802,5.45);
#4476=VECTOR('',#15807,10.);
#4477=VECTOR('',#15808,10.);
#4478=VECTOR('',#15809,10.);
#4479=VECTOR('',#15810,10.);
#4480=VECTOR('',#15827,5.2);
#4481=VECTOR('',#15830,10.);
#4482=VECTOR('',#15831,10.);
#4483=VECTOR('',#15832,10.);
#4484=VECTOR('',#15835,10.);
#4485=VECTOR('',#15842,10.);
#4486=VECTOR('',#15843,10.);
#4487=VECTOR('',#15844,10.);
#4488=VECTOR('',#15847,10.);
#4489=VECTOR('',#15854,10.);
#4490=VECTOR('',#15855,10.);
#4491=VECTOR('',#15856,10.);
#4492=VECTOR('',#15859,10.);
#4493=VECTOR('',#15866,10.);
#4494=VECTOR('',#15867,10.);
#4495=VECTOR('',#15878,10.);
#4496=VECTOR('',#15885,10.);
#4497=VECTOR('',#15888,10.);
#4498=VECTOR('',#15891,10.);
#4499=VECTOR('',#15894,10.);
#4500=VECTOR('',#15899,8.25);
#4501=VECTOR('',#15906,8.);
#4502=VECTOR('',#15909,5.45);
#4503=VECTOR('',#15916,5.2);
#4504=VECTOR('',#15919,5.45);
#4505=VECTOR('',#15926,5.2);
#4506=VECTOR('',#15929,5.45);
#4507=VECTOR('',#15936,5.2);
#4508=VECTOR('',#15939,5.45);
#4509=VECTOR('',#15946,5.2);
#4510=VECTOR('',#15949,5.45);
#4511=VECTOR('',#15956,5.2);
#4512=VECTOR('',#15961,8.25);
#4513=VECTOR('',#15964,10.);
#4514=VECTOR('',#15965,10.);
#4515=VECTOR('',#15966,10.);
#4516=VECTOR('',#15967,10.);
#4517=VECTOR('',#15982,5.45);
#4518=VECTOR('',#15985,5.45);
#4519=VECTOR('',#15988,5.45);
#4520=VECTOR('',#15991,5.45);
#4521=VECTOR('',#15994,5.45);
#4522=VECTOR('',#15997,5.45);
#4523=VECTOR('',#16000,10.);
#4524=VECTOR('',#16001,10.);
#4525=VECTOR('',#16002,10.);
#4526=VECTOR('',#16005,10.);
#4527=VECTOR('',#16010,10.);
#4528=VECTOR('',#16011,10.);
#4529=VECTOR('',#16014,10.);
#4530=VECTOR('',#16019,10.);
#4531=VECTOR('',#16020,10.);
#4532=VECTOR('',#16023,10.);
#4533=VECTOR('',#16028,10.);
#4534=VECTOR('',#16037,10.);
#4535=VECTOR('',#16040,10.);
#4536=VECTOR('',#16045,10.);
#4537=VECTOR('',#16046,10.);
#4538=VECTOR('',#16061,5.45);
#4539=VECTOR('',#16064,5.45);
#4540=VECTOR('',#16067,5.45);
#4541=VECTOR('',#16070,5.45);
#4542=VECTOR('',#16073,5.45);
#4543=VECTOR('',#16076,5.45);
#4544=VECTOR('',#16079,10.);
#4545=VECTOR('',#16080,10.);
#4546=VECTOR('',#16081,10.);
#4547=VECTOR('',#16084,10.);
#4548=VECTOR('',#16089,10.);
#4549=VECTOR('',#16090,10.);
#4550=VECTOR('',#16093,10.);
#4551=VECTOR('',#16100,10.);
#4552=VECTOR('',#16101,10.);
#4553=VECTOR('',#16102,10.);
#4554=VECTOR('',#16105,10.);
#4555=VECTOR('',#16112,10.);
#4556=VECTOR('',#16113,10.);
#4557=VECTOR('',#16114,10.);
#4558=VECTOR('',#16121,10.);
#4559=VECTOR('',#16124,10.);
#4560=VECTOR('',#16127,10.);
#4561=VECTOR('',#16130,10.);
#4562=VECTOR('',#16133,10.);
#4563=VECTOR('',#16138,10.);
#4564=VECTOR('',#16139,10.);
#4565=VECTOR('',#16142,10.);
#4566=VECTOR('',#16145,10.);
#4567=VECTOR('',#16148,10.);
#4568=VECTOR('',#16153,10.);
#4569=VECTOR('',#16154,10.);
#4570=VECTOR('',#16157,10.);
#4571=VECTOR('',#16162,10.);
#4572=VECTOR('',#16163,10.);
#4573=VECTOR('',#16168,10.);
#4574=VECTOR('',#16171,10.);
#4575=VECTOR('',#16174,10.);
#4576=VECTOR('',#16179,10.);
#4577=VECTOR('',#16182,10.);
#4578=VECTOR('',#16187,10.);
#4579=VECTOR('',#16188,10.);
#4580=VECTOR('',#16189,10.);
#4581=VECTOR('',#16192,10.);
#4582=VECTOR('',#16195,10.);
#4583=VECTOR('',#16198,10.);
#4584=VECTOR('',#16201,10.);
#4585=VECTOR('',#16202,10.);
#4586=VECTOR('',#16205,10.);
#4587=VECTOR('',#16206,10.);
#4588=VECTOR('',#16207,10.);
#4589=VECTOR('',#16208,10.);
#4590=VECTOR('',#16211,10.);
#4591=VECTOR('',#16214,10.);
#4592=VECTOR('',#16215,10.);
#4593=VECTOR('',#16216,10.);
#4594=VECTOR('',#16219,10.);
#4595=VECTOR('',#16222,10.);
#4596=VECTOR('',#16225,10.);
#4597=VECTOR('',#16228,10.);
#4598=VECTOR('',#16229,10.);
#4599=VECTOR('',#16230,10.);
#4600=VECTOR('',#16231,10.);
#4601=VECTOR('',#16232,10.);
#4602=VECTOR('',#16235,10.);
#4603=VECTOR('',#16240,10.);
#4604=VECTOR('',#16243,10.);
#4605=VECTOR('',#16244,10.);
#4606=VECTOR('',#16245,10.);
#4607=VECTOR('',#16248,10.);
#4608=VECTOR('',#16251,10.);
#4609=VECTOR('',#16252,10.);
#4610=VECTOR('',#16255,10.);
#4611=VECTOR('',#16256,10.);
#4612=VECTOR('',#16259,10.);
#4613=VECTOR('',#16260,10.);
#4614=VECTOR('',#16261,10.);
#4615=VECTOR('',#16262,10.);
#4616=VECTOR('',#16265,10.);
#4617=VECTOR('',#16268,10.);
#4618=VECTOR('',#16271,10.);
#4619=VECTOR('',#16274,10.);
#4620=VECTOR('',#16277,10.);
#4621=VECTOR('',#16280,10.);
#4622=VECTOR('',#16289,10.);
#4623=VECTOR('',#16292,10.);
#4624=VECTOR('',#16295,10.);
#4625=VECTOR('',#16298,10.);
#4626=VECTOR('',#16305,10.);
#4627=VECTOR('',#16306,10.);
#4628=VECTOR('',#16307,10.);
#4629=VECTOR('',#16310,10.);
#4630=VECTOR('',#16311,10.);
#4631=VECTOR('',#16312,10.);
#4632=VECTOR('',#16315,10.);
#4633=VECTOR('',#16316,10.);
#4634=VECTOR('',#16317,10.);
#4635=VECTOR('',#16318,10.);
#4636=VECTOR('',#16319,10.);
#4637=VECTOR('',#16320,10.);
#4638=VECTOR('',#16321,10.);
#4639=VECTOR('',#16324,10.);
#4640=VECTOR('',#16327,10.);
#4641=VECTOR('',#16328,10.);
#4642=VECTOR('',#16331,10.);
#4643=VECTOR('',#16332,10.);
#4644=VECTOR('',#16333,10.);
#4645=VECTOR('',#16336,10.);
#4646=VECTOR('',#16337,10.);
#4647=VECTOR('',#16338,10.);
#4648=VECTOR('',#16339,10.);
#4649=VECTOR('',#16342,10.);
#4650=VECTOR('',#16343,10.);
#4651=VECTOR('',#16344,10.);
#4652=VECTOR('',#16347,10.);
#4653=VECTOR('',#16350,10.);
#4654=VECTOR('',#16351,10.);
#4655=VECTOR('',#16354,10.);
#4656=VECTOR('',#16357,10.);
#4657=VECTOR('',#16358,10.);
#4658=VECTOR('',#16359,10.);
#4659=VECTOR('',#16360,10.);
#4660=VECTOR('',#16363,10.);
#4661=VECTOR('',#16364,10.);
#4662=VECTOR('',#16367,10.);
#4663=VECTOR('',#16370,10.);
#4664=VECTOR('',#16375,10.);
#4665=VECTOR('',#16378,10.);
#4666=VECTOR('',#16387,10.);
#4667=VECTOR('',#16392,10.);
#4668=VECTOR('',#16393,10.);
#4669=VECTOR('',#16394,10.);
#4670=VECTOR('',#16403,10.);
#4671=VECTOR('',#16404,10.);
#4672=VECTOR('',#16407,10.);
#4673=VECTOR('',#16414,10.);
#4674=VECTOR('',#16415,10.);
#4675=VECTOR('',#16420,10.);
#4676=VECTOR('',#16425,10.);
#4677=VECTOR('',#16432,5.1);
#4678=VECTOR('',#16439,10.);
#4679=VECTOR('',#16442,10.);
#4680=VECTOR('',#16445,10.);
#4681=VECTOR('',#16448,10.);
#4682=VECTOR('',#16451,4.85);
#4683=VECTOR('',#16458,10.);
#4684=VECTOR('',#16463,10.);
#4685=VECTOR('',#16464,10.);
#4686=VECTOR('',#16465,10.);
#4687=VECTOR('',#16474,10.);
#4688=VECTOR('',#16475,10.);
#4689=VECTOR('',#16478,10.);
#4690=VECTOR('',#16485,10.);
#4691=VECTOR('',#16486,10.);
#4692=VECTOR('',#16491,10.);
#4693=VECTOR('',#16496,10.);
#4694=VECTOR('',#16501,10.);
#4695=VECTOR('',#16502,10.);
#4696=VECTOR('',#16503,10.);
#4697=VECTOR('',#16506,10.);
#4698=VECTOR('',#16513,10.);
#4699=VECTOR('',#16514,10.);
#4700=VECTOR('',#16515,10.);
#4701=VECTOR('',#16518,10.);
#4702=VECTOR('',#16525,10.);
#4703=VECTOR('',#16526,10.);
#4704=VECTOR('',#16529,10.);
#4705=VECTOR('',#16530,10.);
#4706=VECTOR('',#16531,10.);
#4707=VECTOR('',#16532,10.);
#4708=VECTOR('',#16533,10.);
#4709=VECTOR('',#16534,10.);
#4710=VECTOR('',#16535,10.);
#4711=VECTOR('',#16536,10.);
#4712=VECTOR('',#16537,10.);
#4713=VECTOR('',#16540,10.);
#4714=VECTOR('',#16545,10.);
#4715=VECTOR('',#16546,10.);
#4716=VECTOR('',#16549,10.);
#4717=VECTOR('',#16554,10.);
#4718=VECTOR('',#16555,10.);
#4719=VECTOR('',#16556,10.);
#4720=VECTOR('',#16557,10.);
#4721=VECTOR('',#16558,10.);
#4722=VECTOR('',#16559,10.);
#4723=VECTOR('',#16560,10.);
#4724=VECTOR('',#16561,10.);
#4725=VECTOR('',#16564,10.);
#4726=VECTOR('',#16565,10.);
#4727=VECTOR('',#16568,10.);
#4728=VECTOR('',#16575,10.);
#4729=VECTOR('',#16576,10.);
#4730=VECTOR('',#16577,10.);
#4731=VECTOR('',#16580,10.);
#4732=VECTOR('',#16587,10.);
#4733=VECTOR('',#16590,10.);
#4734=VECTOR('',#16595,10.);
#4735=VECTOR('',#16596,10.);
#4736=VECTOR('',#16603,10.);
#4737=VECTOR('',#16604,10.);
#4738=VECTOR('',#16609,10.);
#4739=VECTOR('',#16612,10.);
#4740=VECTOR('',#16615,10.);
#4741=VECTOR('',#16618,10.);
#4742=VECTOR('',#16621,10.);
#4743=VECTOR('',#16624,10.);
#4744=VECTOR('',#16629,10.);
#4745=VECTOR('',#16632,10.);
#4746=VECTOR('',#16637,10.);
#4747=VECTOR('',#16638,10.);
#4748=VECTOR('',#16639,10.);
#4749=VECTOR('',#16642,10.);
#4750=VECTOR('',#16643,10.);
#4751=VECTOR('',#16644,10.);
#4752=VECTOR('',#16647,10.);
#4753=VECTOR('',#16648,10.);
#4754=VECTOR('',#16651,10.);
#4755=VECTOR('',#16654,10.);
#4756=VECTOR('',#16657,10.);
#4757=VECTOR('',#16658,10.);
#4758=VECTOR('',#16661,10.);
#4759=VECTOR('',#16666,10.);
#4760=VECTOR('',#16667,10.);
#4761=VECTOR('',#16668,10.);
#4762=VECTOR('',#16671,10.);
#4763=VECTOR('',#16676,10.);
#4764=VECTOR('',#16677,10.);
#4765=VECTOR('',#16680,10.);
#4766=VECTOR('',#16685,10.);
#4767=VECTOR('',#16686,10.);
#4768=VECTOR('',#16689,10.);
#4769=VECTOR('',#16692,10.);
#4770=VECTOR('',#16693,10.);
#4771=VECTOR('',#16694,10.);
#4772=VECTOR('',#16695,10.);
#4773=VECTOR('',#16696,10.);
#4774=VECTOR('',#16697,10.);
#4775=VECTOR('',#16698,10.);
#4776=VECTOR('',#16699,10.);
#4777=VECTOR('',#16700,10.);
#4778=VECTOR('',#16701,10.);
#4779=VECTOR('',#16702,10.);
#4780=VECTOR('',#16703,10.);
#4781=VECTOR('',#16704,10.);
#4782=VECTOR('',#16705,10.);
#4783=VECTOR('',#16706,10.);
#4784=VECTOR('',#16707,10.);
#4785=VECTOR('',#16710,10.);
#4786=VECTOR('',#16711,10.);
#4787=VECTOR('',#16714,10.);
#4788=VECTOR('',#16721,10.);
#4789=VECTOR('',#16722,10.);
#4790=VECTOR('',#16723,10.);
#4791=VECTOR('',#16726,10.);
#4792=VECTOR('',#16731,10.);
#4793=VECTOR('',#16736,10.);
#4794=VECTOR('',#16737,10.);
#4795=VECTOR('',#16740,10.);
#4796=VECTOR('',#16745,10.);
#4797=VECTOR('',#16746,10.);
#4798=VECTOR('',#16749,10.);
#4799=VECTOR('',#16754,10.);
#4800=VECTOR('',#16759,10.);
#4801=VECTOR('',#16760,10.);
#4802=VECTOR('',#16761,10.);
#4803=VECTOR('',#16764,10.);
#4804=VECTOR('',#16765,10.);
#4805=VECTOR('',#16766,10.);
#4806=VECTOR('',#16769,10.);
#4807=VECTOR('',#16772,10.);
#4808=VECTOR('',#16775,10.);
#4809=VECTOR('',#16776,10.);
#4810=VECTOR('',#16777,10.);
#4811=VECTOR('',#16780,10.);
#4812=VECTOR('',#16781,10.);
#4813=VECTOR('',#16786,10.);
#4814=VECTOR('',#16787,10.);
#4815=VECTOR('',#16788,10.);
#4816=VECTOR('',#16791,10.);
#4817=VECTOR('',#16792,10.);
#4818=VECTOR('',#16793,10.);
#4819=VECTOR('',#16796,10.);
#4820=VECTOR('',#16799,10.);
#4821=VECTOR('',#16802,10.);
#4822=VECTOR('',#16803,10.);
#4823=VECTOR('',#16804,10.);
#4824=VECTOR('',#16807,10.);
#4825=VECTOR('',#16808,10.);
#4826=VECTOR('',#16813,10.);
#4827=VECTOR('',#16814,10.);
#4828=VECTOR('',#16815,10.);
#4829=VECTOR('',#16818,10.);
#4830=VECTOR('',#16819,10.);
#4831=VECTOR('',#16820,10.);
#4832=VECTOR('',#16823,10.);
#4833=VECTOR('',#16826,10.);
#4834=VECTOR('',#16829,10.);
#4835=VECTOR('',#16830,10.);
#4836=VECTOR('',#16831,10.);
#4837=VECTOR('',#16834,10.);
#4838=VECTOR('',#16835,10.);
#4839=VECTOR('',#16840,10.);
#4840=VECTOR('',#16841,10.);
#4841=VECTOR('',#16842,10.);
#4842=VECTOR('',#16845,10.);
#4843=VECTOR('',#16846,10.);
#4844=VECTOR('',#16847,10.);
#4845=VECTOR('',#16850,10.);
#4846=VECTOR('',#16853,10.);
#4847=VECTOR('',#16856,10.);
#4848=VECTOR('',#16857,10.);
#4849=VECTOR('',#16858,10.);
#4850=VECTOR('',#16861,10.);
#4851=VECTOR('',#16862,10.);
#4852=VECTOR('',#16867,1.525);
#4853=VECTOR('',#16872,1.525);
#4854=VECTOR('',#16877,1.525);
#4855=VECTOR('',#16882,1.525);
#4856=VECTOR('',#16887,1.525);
#4857=VECTOR('',#16890,10.);
#4858=VECTOR('',#16891,10.);
#4859=VECTOR('',#16894,10.);
#4860=VECTOR('',#16899,10.);
#4861=VECTOR('',#16900,10.);
#4862=VECTOR('',#16903,10.);
#4863=VECTOR('',#16908,10.);
#4864=VECTOR('',#16909,10.);
#4865=VECTOR('',#16912,10.);
#4866=VECTOR('',#16917,10.);
#4867=VECTOR('',#16918,10.);
#4868=VECTOR('',#16921,10.);
#4869=VECTOR('',#16926,10.);
#4870=VECTOR('',#16937,10.);
#4871=VECTOR('',#16948,3.89435028842544);
#4872=VECTOR('',#16955,4.35);
#4873=VECTOR('',#16964,4.61564971157455);
#4874=VECTOR('',#16971,4.75);
#4875=VECTOR('',#16980,4.5);
#4876=VECTOR('',#16991,1.35);
#4877=VECTOR('',#16996,1.5);
#4878=VECTOR('',#17001,1.35);
#4879=VECTOR('',#17008,10.);
#4880=VECTOR('',#17009,10.);
#4881=VECTOR('',#17010,10.);
#4882=VECTOR('',#17011,10.);
#4883=VECTOR('',#17014,10.);
#4884=VECTOR('',#17015,10.);
#4885=VECTOR('',#17016,10.);
#4886=VECTOR('',#17019,10.);
#4887=VECTOR('',#17020,10.);
#4888=VECTOR('',#17021,10.);
#4889=VECTOR('',#17024,10.);
#4890=VECTOR('',#17025,10.);
#4891=VECTOR('',#17026,10.);
#4892=VECTOR('',#17029,10.);
#4893=VECTOR('',#17030,10.);
#4894=VECTOR('',#17031,10.);
#4895=VECTOR('',#17034,10.);
#4896=VECTOR('',#17035,10.);
#4897=VECTOR('',#17036,10.);
#4898=VECTOR('',#17039,10.);
#4899=VECTOR('',#17040,10.);
#4900=VECTOR('',#17041,10.);
#4901=VECTOR('',#17044,10.);
#4902=VECTOR('',#17045,10.);
#4903=VECTOR('',#17046,10.);
#4904=VECTOR('',#17049,10.);
#4905=VECTOR('',#17050,10.);
#4906=VECTOR('',#17051,10.);
#4907=VECTOR('',#17054,10.);
#4908=VECTOR('',#17055,10.);
#4909=VECTOR('',#17056,10.);
#4910=VECTOR('',#17059,10.);
#4911=VECTOR('',#17060,10.);
#4912=VECTOR('',#17061,10.);
#4913=VECTOR('',#17064,10.);
#4914=VECTOR('',#17065,10.);
#4915=VECTOR('',#17066,10.);
#4916=VECTOR('',#17069,10.);
#4917=VECTOR('',#17070,10.);
#4918=VECTOR('',#17071,10.);
#4919=VECTOR('',#17074,10.);
#4920=VECTOR('',#17075,10.);
#4921=VECTOR('',#17076,10.);
#4922=VECTOR('',#17079,10.);
#4923=VECTOR('',#17080,10.);
#4924=VECTOR('',#17081,10.);
#4925=VECTOR('',#17084,10.);
#4926=VECTOR('',#17085,10.);
#4927=VECTOR('',#17086,10.);
#4928=VECTOR('',#17089,10.);
#4929=VECTOR('',#17090,10.);
#4930=VECTOR('',#17091,10.);
#4931=VECTOR('',#17094,10.);
#4932=VECTOR('',#17095,10.);
#4933=VECTOR('',#17096,10.);
#4934=VECTOR('',#17099,10.);
#4935=VECTOR('',#17100,10.);
#4936=VECTOR('',#17101,10.);
#4937=VECTOR('',#17104,10.);
#4938=VECTOR('',#17105,10.);
#4939=VECTOR('',#17106,10.);
#4940=VECTOR('',#17109,10.);
#4941=VECTOR('',#17110,10.);
#4942=VECTOR('',#17111,10.);
#4943=VECTOR('',#17114,10.);
#4944=VECTOR('',#17115,10.);
#4945=VECTOR('',#17116,10.);
#4946=VECTOR('',#17119,10.);
#4947=VECTOR('',#17120,10.);
#4948=VECTOR('',#17121,10.);
#4949=VECTOR('',#17124,10.);
#4950=VECTOR('',#17125,10.);
#4951=VECTOR('',#17126,10.);
#4952=VECTOR('',#17129,10.);
#4953=VECTOR('',#17130,10.);
#4954=VECTOR('',#17131,10.);
#4955=VECTOR('',#17134,10.);
#4956=VECTOR('',#17135,10.);
#4957=VECTOR('',#17136,10.);
#4958=VECTOR('',#17139,10.);
#4959=VECTOR('',#17140,10.);
#4960=VECTOR('',#17141,10.);
#4961=VECTOR('',#17144,10.);
#4962=VECTOR('',#17145,10.);
#4963=VECTOR('',#17146,10.);
#4964=VECTOR('',#17149,10.);
#4965=VECTOR('',#17150,10.);
#4966=VECTOR('',#17151,10.);
#4967=VECTOR('',#17154,10.);
#4968=VECTOR('',#17155,10.);
#4969=VECTOR('',#17156,10.);
#4970=VECTOR('',#17159,10.);
#4971=VECTOR('',#17160,10.);
#4972=VECTOR('',#17161,10.);
#4973=VECTOR('',#17164,10.);
#4974=VECTOR('',#17165,10.);
#4975=VECTOR('',#17166,10.);
#4976=VECTOR('',#17169,10.);
#4977=VECTOR('',#17170,10.);
#4978=VECTOR('',#17171,10.);
#4979=VECTOR('',#17174,10.);
#4980=VECTOR('',#17175,10.);
#4981=VECTOR('',#17176,10.);
#4982=VECTOR('',#17179,10.);
#4983=VECTOR('',#17180,10.);
#4984=VECTOR('',#17181,10.);
#4985=VECTOR('',#17184,10.);
#4986=VECTOR('',#17185,10.);
#4987=VECTOR('',#17186,10.);
#4988=VECTOR('',#17189,10.);
#4989=VECTOR('',#17190,10.);
#4990=VECTOR('',#17191,10.);
#4991=VECTOR('',#17194,10.);
#4992=VECTOR('',#17195,10.);
#4993=VECTOR('',#17196,10.);
#4994=VECTOR('',#17199,10.);
#4995=VECTOR('',#17200,10.);
#4996=VECTOR('',#17201,10.);
#4997=VECTOR('',#17204,10.);
#4998=VECTOR('',#17205,10.);
#4999=VECTOR('',#17206,10.);
#5000=VECTOR('',#17209,10.);
#5001=VECTOR('',#17210,10.);
#5002=VECTOR('',#17211,10.);
#5003=VECTOR('',#17214,10.);
#5004=VECTOR('',#17215,10.);
#5005=VECTOR('',#17216,10.);
#5006=VECTOR('',#17219,10.);
#5007=VECTOR('',#17220,10.);
#5008=VECTOR('',#17221,10.);
#5009=VECTOR('',#17224,10.);
#5010=VECTOR('',#17225,10.);
#5011=VECTOR('',#17226,10.);
#5012=VECTOR('',#17229,10.);
#5013=VECTOR('',#17230,10.);
#5014=VECTOR('',#17231,10.);
#5015=VECTOR('',#17234,10.);
#5016=VECTOR('',#17235,10.);
#5017=VECTOR('',#17236,10.);
#5018=VECTOR('',#17239,10.);
#5019=VECTOR('',#17240,10.);
#5020=VECTOR('',#17241,10.);
#5021=VECTOR('',#17244,10.);
#5022=VECTOR('',#17245,10.);
#5023=VECTOR('',#17246,10.);
#5024=VECTOR('',#17249,10.);
#5025=VECTOR('',#17250,10.);
#5026=VECTOR('',#17251,10.);
#5027=VECTOR('',#17254,10.);
#5028=VECTOR('',#17255,10.);
#5029=VECTOR('',#17264,10.);
#5030=VECTOR('',#17265,10.);
#5031=VECTOR('',#17266,10.);
#5032=VECTOR('',#17267,10.);
#5033=VECTOR('',#17270,10.);
#5034=VECTOR('',#17277,10.);
#5035=VECTOR('',#17278,10.);
#5036=VECTOR('',#17279,10.);
#5037=VECTOR('',#17282,10.);
#5038=VECTOR('',#17289,10.);
#5039=VECTOR('',#17290,10.);
#5040=VECTOR('',#17291,10.);
#5041=VECTOR('',#17294,10.);
#5042=VECTOR('',#17301,10.);
#5043=VECTOR('',#17302,10.);
#5044=VECTOR('',#17303,10.);
#5045=VECTOR('',#17312,10.);
#5046=VECTOR('',#17315,10.);
#5047=VECTOR('',#17318,10.);
#5048=VECTOR('',#17319,10.);
#5049=VECTOR('',#17322,10.);
#5050=VECTOR('',#17327,10.);
#5051=VECTOR('',#17328,10.);
#5052=VECTOR('',#17331,10.);
#5053=VECTOR('',#17334,10.);
#5054=VECTOR('',#17337,10.);
#5055=VECTOR('',#17340,10.);
#5056=VECTOR('',#17345,10.);
#5057=VECTOR('',#17348,10.);
#5058=VECTOR('',#17353,10.);
#5059=VECTOR('',#17354,10.);
#5060=VECTOR('',#17355,10.);
#5061=VECTOR('',#17358,10.);
#5062=VECTOR('',#17365,10.);
#5063=VECTOR('',#17366,10.);
#5064=VECTOR('',#17367,10.);
#5065=VECTOR('',#17370,10.);
#5066=VECTOR('',#17377,10.);
#5067=VECTOR('',#17378,10.);
#5068=VECTOR('',#17379,10.);
#5069=VECTOR('',#17382,10.);
#5070=VECTOR('',#17389,10.);
#5071=VECTOR('',#17390,10.);
#5072=VECTOR('',#17393,10.);
#5073=VECTOR('',#17394,10.);
#5074=VECTOR('',#17397,10.);
#5075=VECTOR('',#17400,10.);
#5076=VECTOR('',#17403,10.);
#5077=VECTOR('',#17408,10.);
#5078=VECTOR('',#17411,10.);
#5079=VECTOR('',#17414,10.);
#5080=VECTOR('',#17417,10.);
#5081=VECTOR('',#17420,10.);
#5082=VECTOR('',#17421,10.);
#5083=VECTOR('',#17426,10.);
#5084=VECTOR('',#17427,10.);
#5085=VECTOR('',#17430,10.);
#5086=VECTOR('',#17435,10.);
#5087=VECTOR('',#17436,10.);
#5088=VECTOR('',#17439,10.);
#5089=VECTOR('',#17444,10.);
#5090=VECTOR('',#17445,10.);
#5091=VECTOR('',#17448,10.);
#5092=VECTOR('',#17453,10.);
#5093=VECTOR('',#17456,10.);
#5094=VECTOR('',#17457,10.);
#5095=VECTOR('',#17458,10.);
#5096=VECTOR('',#17459,10.);
#5097=VECTOR('',#17460,10.);
#5098=VECTOR('',#17463,10.);
#5099=VECTOR('',#17468,10.);
#5100=VECTOR('',#17469,10.);
#5101=VECTOR('',#17470,10.);
#5102=VECTOR('',#17471,10.);
#5103=VECTOR('',#17474,10.);
#5104=VECTOR('',#17477,10.);
#5105=VECTOR('',#17478,10.);
#5106=VECTOR('',#17481,10.);
#5107=VECTOR('',#17484,10.);
#5108=VECTOR('',#17487,10.);
#5109=VECTOR('',#17490,10.);
#5110=VECTOR('',#17493,10.);
#5111=VECTOR('',#17494,10.);
#5112=VECTOR('',#17495,10.);
#5113=VECTOR('',#17496,10.);
#5114=VECTOR('',#17499,10.);
#5115=VECTOR('',#17502,10.);
#5116=VECTOR('',#17505,10.);
#5117=VECTOR('',#17508,10.);
#5118=VECTOR('',#17509,10.);
#5119=VECTOR('',#17512,10.);
#5120=VECTOR('',#17515,10.);
#5121=VECTOR('',#17518,10.);
#5122=VECTOR('',#17521,10.);
#5123=VECTOR('',#17524,10.);
#5124=VECTOR('',#17525,10.);
#5125=VECTOR('',#17528,10.);
#5126=VECTOR('',#17533,10.);
#5127=VECTOR('',#17534,10.);
#5128=VECTOR('',#17537,10.);
#5129=VECTOR('',#17544,10.);
#5130=VECTOR('',#17545,10.);
#5131=VECTOR('',#17546,10.);
#5132=VECTOR('',#17549,10.);
#5133=VECTOR('',#17556,10.);
#5134=VECTOR('',#17557,10.);
#5135=VECTOR('',#17562,10.);
#5136=VECTOR('',#17565,10.);
#5137=VECTOR('',#17566,10.);
#5138=VECTOR('',#17569,10.);
#5139=VECTOR('',#17570,10.);
#5140=VECTOR('',#17571,10.);
#5141=VECTOR('',#17574,10.);
#5142=VECTOR('',#17575,10.);
#5143=VECTOR('',#17578,10.);
#5144=VECTOR('',#17579,10.);
#5145=VECTOR('',#17580,10.);
#5146=VECTOR('',#17583,10.);
#5147=VECTOR('',#17588,10.);
#5148=VECTOR('',#17591,10.);
#5149=VECTOR('',#17594,10.);
#5150=VECTOR('',#17599,10.);
#5151=VECTOR('',#17600,10.);
#5152=VECTOR('',#17603,10.);
#5153=VECTOR('',#17612,10.);
#5154=VECTOR('',#17613,10.);
#5155=VECTOR('',#17614,10.);
#5156=VECTOR('',#17615,10.);
#5157=VECTOR('',#17616,10.);
#5158=VECTOR('',#17617,10.);
#5159=VECTOR('',#17620,10.);
#5160=VECTOR('',#17627,10.);
#5161=VECTOR('',#17628,10.);
#5162=VECTOR('',#17629,10.);
#5163=VECTOR('',#17632,10.);
#5164=VECTOR('',#17639,10.);
#5165=VECTOR('',#17640,10.);
#5166=VECTOR('',#17641,10.);
#5167=VECTOR('',#17644,10.);
#5168=VECTOR('',#17651,10.);
#5169=VECTOR('',#17652,10.);
#5170=VECTOR('',#17653,10.);
#5171=VECTOR('',#17662,10.);
#5172=VECTOR('',#17663,10.);
#5173=VECTOR('',#17664,10.);
#5174=VECTOR('',#17667,10.);
#5175=VECTOR('',#17670,10.);
#5176=VECTOR('',#17673,10.);
#5177=VECTOR('',#17676,10.);
#5178=VECTOR('',#17677,10.);
#5179=VECTOR('',#17678,10.);
#5180=VECTOR('',#17681,10.);
#5181=VECTOR('',#17684,10.);
#5182=VECTOR('',#17687,10.);
#5183=VECTOR('',#17688,10.);
#5184=VECTOR('',#17691,10.);
#5185=VECTOR('',#17696,10.);
#5186=VECTOR('',#17697,10.);
#5187=VECTOR('',#17700,10.);
#5188=VECTOR('',#17701,10.);
#5189=VECTOR('',#17702,10.);
#5190=VECTOR('',#17705,10.);
#5191=VECTOR('',#17706,10.);
#5192=VECTOR('',#17707,10.);
#5193=VECTOR('',#17708,10.);
#5194=VECTOR('',#17711,10.);
#5195=VECTOR('',#17712,10.);
#5196=VECTOR('',#17713,10.);
#5197=VECTOR('',#17714,10.);
#5198=VECTOR('',#17717,10.);
#5199=VECTOR('',#17718,10.);
#5200=VECTOR('',#17721,10.);
#5201=VECTOR('',#17722,10.);
#5202=VECTOR('',#17725,10.);
#5203=VECTOR('',#17726,10.);
#5204=VECTOR('',#17727,10.);
#5205=VECTOR('',#17730,10.);
#5206=VECTOR('',#17731,10.);
#5207=VECTOR('',#17734,10.);
#5208=VECTOR('',#17735,10.);
#5209=VECTOR('',#17736,10.);
#5210=VECTOR('',#17739,10.);
#5211=VECTOR('',#17742,10.);
#5212=VECTOR('',#17745,10.);
#5213=VECTOR('',#17748,10.);
#5214=VECTOR('',#17749,10.);
#5215=VECTOR('',#17752,10.);
#5216=VECTOR('',#17753,10.);
#5217=VECTOR('',#17754,10.);
#5218=VECTOR('',#17755,10.);
#5219=VECTOR('',#17758,10.);
#5220=VECTOR('',#17761,10.);
#5221=VECTOR('',#17762,10.);
#5222=VECTOR('',#17765,10.);
#5223=VECTOR('',#17768,10.);
#5224=VECTOR('',#17771,10.);
#5225=VECTOR('',#17774,10.);
#5226=VECTOR('',#17777,10.);
#5227=VECTOR('',#17780,10.);
#5228=VECTOR('',#17783,10.);
#5229=VECTOR('',#17784,10.);
#5230=VECTOR('',#17787,10.);
#5231=VECTOR('',#17788,10.);
#5232=VECTOR('',#17791,10.);
#5233=VECTOR('',#17792,10.);
#5234=VECTOR('',#17793,10.);
#5235=VECTOR('',#17796,10.);
#5236=VECTOR('',#17801,10.);
#5237=VECTOR('',#17802,10.);
#5238=VECTOR('',#17805,10.);
#5239=VECTOR('',#17810,10.);
#5240=VECTOR('',#17813,10.);
#5241=VECTOR('',#17816,10.);
#5242=VECTOR('',#17817,10.);
#5243=VECTOR('',#17820,10.);
#5244=VECTOR('',#17825,10.);
#5245=VECTOR('',#17826,10.);
#5246=VECTOR('',#17829,10.);
#5247=VECTOR('',#17830,10.);
#5248=VECTOR('',#17833,10.);
#5249=VECTOR('',#17834,10.);
#5250=VECTOR('',#17837,10.);
#5251=VECTOR('',#17840,10.);
#5252=VECTOR('',#17841,10.);
#5253=VECTOR('',#17842,10.);
#5254=VECTOR('',#17845,10.);
#5255=VECTOR('',#17852,10.);
#5256=VECTOR('',#17853,10.);
#5257=VECTOR('',#17854,10.);
#5258=VECTOR('',#17857,10.);
#5259=VECTOR('',#17860,10.);
#5260=VECTOR('',#17861,10.);
#5261=VECTOR('',#17864,10.);
#5262=VECTOR('',#17867,10.);
#5263=VECTOR('',#17870,10.);
#5264=VECTOR('',#17871,10.);
#5265=VECTOR('',#17872,10.);
#5266=VECTOR('',#17875,10.);
#5267=VECTOR('',#17876,10.);
#5268=VECTOR('',#17877,10.);
#5269=VECTOR('',#17882,10.);
#5270=VECTOR('',#17887,10.);
#5271=VECTOR('',#17892,10.);
#5272=VECTOR('',#17893,10.);
#5273=VECTOR('',#17896,10.);
#5274=VECTOR('',#17901,10.);
#5275=VECTOR('',#17910,1.72);
#5276=VECTOR('',#17917,1.6);
#5277=VECTOR('',#17920,10.);
#5278=VECTOR('',#17921,10.);
#5279=VECTOR('',#17922,10.);
#5280=VECTOR('',#17923,10.);
#5281=VECTOR('',#17924,10.);
#5282=VECTOR('',#17925,10.);
#5283=VECTOR('',#17926,10.);
#5284=VECTOR('',#17927,10.);
#5285=VECTOR('',#17928,10.);
#5286=VECTOR('',#17929,10.);
#5287=VECTOR('',#17934,1.72);
#5288=VECTOR('',#17937,10.);
#5289=VECTOR('',#17938,10.);
#5290=VECTOR('',#17939,10.);
#5291=VECTOR('',#17940,10.);
#5292=VECTOR('',#17941,10.);
#5293=VECTOR('',#17942,10.);
#5294=VECTOR('',#17943,10.);
#5295=VECTOR('',#17944,10.);
#5296=VECTOR('',#17945,10.);
#5297=VECTOR('',#17946,10.);
#5298=VECTOR('',#17947,10.);
#5299=VECTOR('',#17948,10.);
#5300=VECTOR('',#17949,10.);
#5301=VECTOR('',#17950,10.);
#5302=VECTOR('',#17951,10.);
#5303=VECTOR('',#17952,10.);
#5304=VECTOR('',#17953,10.);
#5305=VECTOR('',#17954,10.);
#5306=VECTOR('',#17955,10.);
#5307=VECTOR('',#17956,10.);
#5308=VECTOR('',#17957,10.);
#5309=VECTOR('',#17958,10.);
#5310=VECTOR('',#17959,10.);
#5311=VECTOR('',#17960,10.);
#5312=VECTOR('',#17961,10.);
#5313=VECTOR('',#17962,10.);
#5314=VECTOR('',#17963,10.);
#5315=VECTOR('',#17964,10.);
#5316=VECTOR('',#17965,10.);
#5317=VECTOR('',#17966,10.);
#5318=VECTOR('',#17967,10.);
#5319=VECTOR('',#17968,10.);
#5320=VECTOR('',#17969,10.);
#5321=VECTOR('',#17970,10.);
#5322=VECTOR('',#17971,10.);
#5323=VECTOR('',#17972,10.);
#5324=VECTOR('',#17973,10.);
#5325=VECTOR('',#17974,10.);
#5326=VECTOR('',#17975,10.);
#5327=VECTOR('',#17976,10.);
#5328=VECTOR('',#17977,10.);
#5329=VECTOR('',#17978,10.);
#5330=VECTOR('',#17979,10.);
#5331=VECTOR('',#17980,10.);
#5332=VECTOR('',#17981,10.);
#5333=VECTOR('',#17982,10.);
#5334=VECTOR('',#17983,10.);
#5335=VECTOR('',#17984,10.);
#5336=VECTOR('',#17985,10.);
#5337=VECTOR('',#17986,10.);
#5338=VECTOR('',#17987,10.);
#5339=VECTOR('',#17988,10.);
#5340=VECTOR('',#17989,10.);
#5341=VECTOR('',#17990,10.);
#5342=VECTOR('',#17991,10.);
#5343=VECTOR('',#17992,10.);
#5344=VECTOR('',#17993,10.);
#5345=VECTOR('',#17994,10.);
#5346=VECTOR('',#17995,10.);
#5347=VECTOR('',#17996,10.);
#5348=VECTOR('',#17999,10.);
#5349=VECTOR('',#18000,10.);
#5350=VECTOR('',#18001,10.);
#5351=VECTOR('',#18004,10.);
#5352=VECTOR('',#18005,10.);
#5353=VECTOR('',#18006,10.);
#5354=VECTOR('',#18009,10.);
#5355=VECTOR('',#18010,10.);
#5356=VECTOR('',#18011,10.);
#5357=VECTOR('',#18014,10.);
#5358=VECTOR('',#18015,10.);
#5359=VECTOR('',#18016,10.);
#5360=VECTOR('',#18019,10.);
#5361=VECTOR('',#18020,10.);
#5362=VECTOR('',#18021,10.);
#5363=VECTOR('',#18024,10.);
#5364=VECTOR('',#18025,10.);
#5365=VECTOR('',#18026,10.);
#5366=VECTOR('',#18029,10.);
#5367=VECTOR('',#18030,10.);
#5368=VECTOR('',#18031,10.);
#5369=VECTOR('',#18034,10.);
#5370=VECTOR('',#18035,10.);
#5371=VECTOR('',#18036,10.);
#5372=VECTOR('',#18039,10.);
#5373=VECTOR('',#18040,10.);
#5374=VECTOR('',#18041,10.);
#5375=VECTOR('',#18044,10.);
#5376=VECTOR('',#18047,10.);
#5377=VECTOR('',#18048,10.);
#5378=VECTOR('',#18049,10.);
#5379=VECTOR('',#18052,10.);
#5380=VECTOR('',#18055,10.);
#5381=VECTOR('',#18056,10.);
#5382=VECTOR('',#18057,10.);
#5383=VECTOR('',#18060,10.);
#5384=VECTOR('',#18061,10.);
#5385=VECTOR('',#18064,10.);
#5386=VECTOR('',#18065,10.);
#5387=VECTOR('',#18068,10.);
#5388=VECTOR('',#18069,10.);
#5389=VECTOR('',#18072,10.);
#5390=VECTOR('',#18073,10.);
#5391=VECTOR('',#18074,10.);
#5392=VECTOR('',#18077,10.);
#5393=VECTOR('',#18078,10.);
#5394=VECTOR('',#18079,10.);
#5395=VECTOR('',#18082,10.);
#5396=VECTOR('',#18083,10.);
#5397=VECTOR('',#18084,10.);
#5398=VECTOR('',#18085,10.);
#5399=VECTOR('',#18088,10.);
#5400=VECTOR('',#18089,10.);
#5401=VECTOR('',#18092,10.);
#5402=VECTOR('',#18093,10.);
#5403=VECTOR('',#18096,10.);
#5404=VECTOR('',#18097,10.);
#5405=VECTOR('',#18098,10.);
#5406=VECTOR('',#18101,10.);
#5407=VECTOR('',#18102,10.);
#5408=VECTOR('',#18103,10.);
#5409=VECTOR('',#18106,10.);
#5410=VECTOR('',#18107,10.);
#5411=VECTOR('',#18108,10.);
#5412=VECTOR('',#18111,10.);
#5413=VECTOR('',#18112,10.);
#5414=VECTOR('',#18113,10.);
#5415=VECTOR('',#18116,10.);
#5416=VECTOR('',#18117,10.);
#5417=VECTOR('',#18118,10.);
#5418=VECTOR('',#18121,10.);
#5419=VECTOR('',#18122,10.);
#5420=VECTOR('',#18123,10.);
#5421=VECTOR('',#18126,10.);
#5422=VECTOR('',#18127,10.);
#5423=VECTOR('',#18128,10.);
#5424=VECTOR('',#18131,10.);
#5425=VECTOR('',#18132,10.);
#5426=VECTOR('',#18133,10.);
#5427=VECTOR('',#18136,10.);
#5428=VECTOR('',#18137,10.);
#5429=VECTOR('',#18138,10.);
#5430=VECTOR('',#18141,10.);
#5431=VECTOR('',#18142,10.);
#5432=VECTOR('',#18143,10.);
#5433=VECTOR('',#18146,10.);
#5434=VECTOR('',#18147,10.);
#5435=VECTOR('',#18148,10.);
#5436=VECTOR('',#18151,10.);
#5437=VECTOR('',#18152,10.);
#5438=VECTOR('',#18153,10.);
#5439=VECTOR('',#18156,10.);
#5440=VECTOR('',#18157,10.);
#5441=VECTOR('',#18160,10.);
#5442=VECTOR('',#18161,10.);
#5443=VECTOR('',#18162,10.);
#5444=VECTOR('',#18165,10.);
#5445=VECTOR('',#18168,10.);
#5446=VECTOR('',#18169,10.);
#5447=VECTOR('',#18170,10.);
#5448=VECTOR('',#18173,10.);
#5449=VECTOR('',#18176,10.);
#5450=VECTOR('',#18177,10.);
#5451=VECTOR('',#18178,10.);
#5452=VECTOR('',#18181,10.);
#5453=VECTOR('',#18184,10.);
#5454=VECTOR('',#18185,10.);
#5455=VECTOR('',#18186,10.);
#5456=VECTOR('',#18189,10.);
#5457=VECTOR('',#18190,10.);
#5458=VECTOR('',#18193,10.);
#5459=VECTOR('',#18194,10.);
#5460=VECTOR('',#18197,10.);
#5461=VECTOR('',#18200,10.);
#5462=VECTOR('',#18201,10.);
#5463=VECTOR('',#18204,10.);
#5464=VECTOR('',#18205,10.);
#5465=VECTOR('',#18208,10.);
#5466=VECTOR('',#18209,10.);
#5467=VECTOR('',#18212,10.);
#5468=VECTOR('',#18213,10.);
#5469=VECTOR('',#18216,10.);
#5470=VECTOR('',#18217,10.);
#5471=VECTOR('',#18220,10.);
#5472=VECTOR('',#18221,10.);
#5473=VECTOR('',#18222,10.);
#5474=VECTOR('',#18225,10.);
#5475=VECTOR('',#18226,10.);
#5476=VECTOR('',#18227,10.);
#5477=VECTOR('',#18230,10.);
#5478=VECTOR('',#18231,10.);
#5479=VECTOR('',#18232,10.);
#5480=VECTOR('',#18235,10.);
#5481=VECTOR('',#18236,10.);
#5482=VECTOR('',#18237,10.);
#5483=VECTOR('',#18240,10.);
#5484=VECTOR('',#18241,10.);
#5485=VECTOR('',#18242,10.);
#5486=VECTOR('',#18245,10.);
#5487=VECTOR('',#18246,10.);
#5488=VECTOR('',#18247,10.);
#5489=VECTOR('',#18250,10.);
#5490=VECTOR('',#18251,10.);
#5491=VECTOR('',#18252,10.);
#5492=VECTOR('',#18255,10.);
#5493=VECTOR('',#18256,10.);
#5494=VECTOR('',#18257,10.);
#5495=VECTOR('',#18260,10.);
#5496=VECTOR('',#18263,10.);
#5497=VECTOR('',#18268,10.);
#5498=VECTOR('',#18269,10.);
#5499=VECTOR('',#18276,10.);
#5500=VECTOR('',#18277,10.);
#5501=VECTOR('',#18284,10.);
#5502=VECTOR('',#18285,10.);
#5503=VECTOR('',#18292,10.);
#5504=VECTOR('',#18293,10.);
#5505=VECTOR('',#18300,10.);
#5506=VECTOR('',#18301,10.);
#5507=VECTOR('',#18308,10.);
#5508=VECTOR('',#18309,10.);
#5509=VECTOR('',#18316,10.);
#5510=VECTOR('',#18317,10.);
#5511=VECTOR('',#18324,10.);
#5512=VECTOR('',#18325,10.);
#5513=VECTOR('',#18332,10.);
#5514=VECTOR('',#18333,10.);
#5515=VECTOR('',#18336,10.);
#5516=VECTOR('',#18337,10.);
#5517=VECTOR('',#18340,10.);
#5518=VERTEX_POINT('',#18380);
#5519=VERTEX_POINT('',#18381);
#5520=VERTEX_POINT('',#18383);
#5521=VERTEX_POINT('',#18385);
#5522=VERTEX_POINT('',#18389);
#5523=VERTEX_POINT('',#18390);
#5524=VERTEX_POINT('',#18395);
#5525=VERTEX_POINT('',#18396);
#5526=VERTEX_POINT('',#18401);
#5527=VERTEX_POINT('',#18402);
#5528=VERTEX_POINT('',#18407);
#5529=VERTEX_POINT('',#18408);
#5530=VERTEX_POINT('',#18413);
#5531=VERTEX_POINT('',#18414);
#5532=VERTEX_POINT('',#18419);
#5533=VERTEX_POINT('',#18420);
#5534=VERTEX_POINT('',#18428);
#5535=VERTEX_POINT('',#18430);
#5536=VERTEX_POINT('',#18434);
#5537=VERTEX_POINT('',#18437);
#5538=VERTEX_POINT('',#18440);
#5539=VERTEX_POINT('',#18444);
#5540=VERTEX_POINT('',#18448);
#5541=VERTEX_POINT('',#18449);
#5542=VERTEX_POINT('',#18451);
#5543=VERTEX_POINT('',#18453);
#5544=VERTEX_POINT('',#18455);
#5545=VERTEX_POINT('',#18457);
#5546=VERTEX_POINT('',#18459);
#5547=VERTEX_POINT('',#18461);
#5548=VERTEX_POINT('',#18465);
#5549=VERTEX_POINT('',#18467);
#5550=VERTEX_POINT('',#18471);
#5551=VERTEX_POINT('',#18475);
#5552=VERTEX_POINT('',#18479);
#5553=VERTEX_POINT('',#18483);
#5554=VERTEX_POINT('',#18487);
#5555=VERTEX_POINT('',#18491);
#5556=VERTEX_POINT('',#18497);
#5557=VERTEX_POINT('',#18499);
#5558=VERTEX_POINT('',#18503);
#5559=VERTEX_POINT('',#18507);
#5560=VERTEX_POINT('',#18511);
#5561=VERTEX_POINT('',#18515);
#5562=VERTEX_POINT('',#18517);
#5563=VERTEX_POINT('',#18521);
#5564=VERTEX_POINT('',#18525);
#5565=VERTEX_POINT('',#18526);
#5566=VERTEX_POINT('',#18531);
#5567=VERTEX_POINT('',#18532);
#5568=VERTEX_POINT('',#18537);
#5569=VERTEX_POINT('',#18538);
#5570=VERTEX_POINT('',#18543);
#5571=VERTEX_POINT('',#18548);
#5572=VERTEX_POINT('',#18556);
#5573=VERTEX_POINT('',#18557);
#5574=VERTEX_POINT('',#18559);
#5575=VERTEX_POINT('',#18561);
#5576=VERTEX_POINT('',#18563);
#5577=VERTEX_POINT('',#18565);
#5578=VERTEX_POINT('',#18567);
#5579=VERTEX_POINT('',#18569);
#5580=VERTEX_POINT('',#18578);
#5581=VERTEX_POINT('',#18582);
#5582=VERTEX_POINT('',#18586);
#5583=VERTEX_POINT('',#18598);
#5584=VERTEX_POINT('',#18632);
#5585=VERTEX_POINT('',#18633);
#5586=VERTEX_POINT('',#18716);
#5587=VERTEX_POINT('',#18721);
#5588=VERTEX_POINT('',#18811);
#5589=VERTEX_POINT('',#18812);
#5590=VERTEX_POINT('',#18865);
#5591=VERTEX_POINT('',#18870);
#5592=VERTEX_POINT('',#18978);
#5593=VERTEX_POINT('',#18985);
#5594=VERTEX_POINT('',#18994);
#5595=VERTEX_POINT('',#18995);
#5596=VERTEX_POINT('',#18997);
#5597=VERTEX_POINT('',#18999);
#5598=VERTEX_POINT('',#19050);
#5599=VERTEX_POINT('',#19057);
#5600=VERTEX_POINT('',#19090);
#5601=VERTEX_POINT('',#19092);
#5602=VERTEX_POINT('',#19175);
#5603=VERTEX_POINT('',#19184);
#5604=VERTEX_POINT('',#19186);
#5605=VERTEX_POINT('',#19188);
#5606=VERTEX_POINT('',#19190);
#5607=VERTEX_POINT('',#19192);
#5608=VERTEX_POINT('',#19196);
#5609=VERTEX_POINT('',#19198);
#5610=VERTEX_POINT('',#19251);
#5611=VERTEX_POINT('',#19258);
#5612=VERTEX_POINT('',#19263);
#5613=VERTEX_POINT('',#19265);
#5614=VERTEX_POINT('',#19270);
#5615=VERTEX_POINT('',#19349);
#5616=VERTEX_POINT('',#19350);
#5617=VERTEX_POINT('',#19433);
#5618=VERTEX_POINT('',#19438);
#5619=VERTEX_POINT('',#19528);
#5620=VERTEX_POINT('',#19609);
#5621=VERTEX_POINT('',#19618);
#5622=VERTEX_POINT('',#19619);
#5623=VERTEX_POINT('',#19621);
#5624=VERTEX_POINT('',#19623);
#5625=VERTEX_POINT('',#19674);
#5626=VERTEX_POINT('',#19681);
#5627=VERTEX_POINT('',#19714);
#5628=VERTEX_POINT('',#19716);
#5629=VERTEX_POINT('',#19718);
#5630=VERTEX_POINT('',#19720);
#5631=VERTEX_POINT('',#19743);
#5632=VERTEX_POINT('',#19826);
#5633=VERTEX_POINT('',#19919);
#5634=VERTEX_POINT('',#19920);
#5635=VERTEX_POINT('',#19973);
#5636=VERTEX_POINT('',#19978);
#5637=VERTEX_POINT('',#20086);
#5638=VERTEX_POINT('',#20093);
#5639=VERTEX_POINT('',#20102);
#5640=VERTEX_POINT('',#20103);
#5641=VERTEX_POINT('',#20105);
#5642=VERTEX_POINT('',#20107);
#5643=VERTEX_POINT('',#20158);
#5644=VERTEX_POINT('',#20165);
#5645=VERTEX_POINT('',#20198);
#5646=VERTEX_POINT('',#20281);
#5647=VERTEX_POINT('',#20311);
#5648=VERTEX_POINT('',#20312);
#5649=VERTEX_POINT('',#20466);
#5650=VERTEX_POINT('',#20468);
#5651=VERTEX_POINT('',#20515);
#5652=VERTEX_POINT('',#20544);
#5653=VERTEX_POINT('',#20546);
#5654=VERTEX_POINT('',#20548);
#5655=VERTEX_POINT('',#20550);
#5656=VERTEX_POINT('',#20554);
#5657=VERTEX_POINT('',#20563);
#5658=VERTEX_POINT('',#20571);
#5659=VERTEX_POINT('',#20578);
#5660=VERTEX_POINT('',#20590);
#5661=VERTEX_POINT('',#20599);
#5662=VERTEX_POINT('',#20607);
#5663=VERTEX_POINT('',#20614);
#5664=VERTEX_POINT('',#20655);
#5665=VERTEX_POINT('',#20656);
#5666=VERTEX_POINT('',#20703);
#5667=VERTEX_POINT('',#20708);
#5668=VERTEX_POINT('',#20780);
#5669=VERTEX_POINT('',#20781);
#5670=VERTEX_POINT('',#20828);
#5671=VERTEX_POINT('',#20833);
#5672=VERTEX_POINT('',#20909);
#5673=VERTEX_POINT('',#20917);
#5674=VERTEX_POINT('',#20927);
#5675=VERTEX_POINT('',#20928);
#5676=VERTEX_POINT('',#20969);
#5677=VERTEX_POINT('',#20971);
#5678=VERTEX_POINT('',#20978);
#5679=VERTEX_POINT('',#21027);
#5680=VERTEX_POINT('',#21031);
#5681=VERTEX_POINT('',#21033);
#5682=VERTEX_POINT('',#21087);
#5683=VERTEX_POINT('',#21089);
#5684=VERTEX_POINT('',#21091);
#5685=VERTEX_POINT('',#21093);
#5686=VERTEX_POINT('',#21095);
#5687=VERTEX_POINT('',#21122);
#5688=VERTEX_POINT('',#21127);
#5689=VERTEX_POINT('',#21199);
#5690=VERTEX_POINT('',#21274);
#5691=VERTEX_POINT('',#21283);
#5692=VERTEX_POINT('',#21317);
#5693=VERTEX_POINT('',#21319);
#5694=VERTEX_POINT('',#21326);
#5695=VERTEX_POINT('',#21375);
#5696=VERTEX_POINT('',#21379);
#5697=VERTEX_POINT('',#21456);
#5698=VERTEX_POINT('',#21531);
#5699=VERTEX_POINT('',#21536);
#5700=VERTEX_POINT('',#21608);
#5701=VERTEX_POINT('',#21617);
#5702=VERTEX_POINT('',#21674);
#5703=VERTEX_POINT('',#21721);
#5704=VERTEX_POINT('',#21796);
#5705=VERTEX_POINT('',#21797);
#5706=VERTEX_POINT('',#21844);
#5707=VERTEX_POINT('',#21849);
#5708=VERTEX_POINT('',#21921);
#5709=VERTEX_POINT('',#21928);
#5710=VERTEX_POINT('',#21937);
#5711=VERTEX_POINT('',#21939);
#5712=VERTEX_POINT('',#21993);
#5713=VERTEX_POINT('',#21995);
#5714=VERTEX_POINT('',#21999);
#5715=VERTEX_POINT('',#22003);
#5716=VERTEX_POINT('',#22004);
#5717=VERTEX_POINT('',#22006);
#5718=VERTEX_POINT('',#22008);
#5719=VERTEX_POINT('',#22012);
#5720=VERTEX_POINT('',#22016);
#5721=VERTEX_POINT('',#22017);
#5722=VERTEX_POINT('',#22019);
#5723=VERTEX_POINT('',#22021);
#5724=VERTEX_POINT('',#22025);
#5725=VERTEX_POINT('',#22026);
#5726=VERTEX_POINT('',#22028);
#5727=VERTEX_POINT('',#22030);
#5728=VERTEX_POINT('',#22034);
#5729=VERTEX_POINT('',#22035);
#5730=VERTEX_POINT('',#22040);
#5731=VERTEX_POINT('',#22041);
#5732=VERTEX_POINT('',#22046);
#5733=VERTEX_POINT('',#22051);
#5734=VERTEX_POINT('',#22055);
#5735=VERTEX_POINT('',#22056);
#5736=VERTEX_POINT('',#22061);
#5737=VERTEX_POINT('',#22062);
#5738=VERTEX_POINT('',#22070);
#5739=VERTEX_POINT('',#22074);
#5740=VERTEX_POINT('',#22078);
#5741=VERTEX_POINT('',#22082);
#5742=VERTEX_POINT('',#22086);
#5743=VERTEX_POINT('',#22087);
#5744=VERTEX_POINT('',#22089);
#5745=VERTEX_POINT('',#22091);
#5746=VERTEX_POINT('',#22093);
#5747=VERTEX_POINT('',#22095);
#5748=VERTEX_POINT('',#22097);
#5749=VERTEX_POINT('',#22099);
#5750=VERTEX_POINT('',#22103);
#5751=VERTEX_POINT('',#22108);
#5752=VERTEX_POINT('',#22112);
#5753=VERTEX_POINT('',#22116);
#5754=VERTEX_POINT('',#22120);
#5755=VERTEX_POINT('',#22124);
#5756=VERTEX_POINT('',#22132);
#5757=VERTEX_POINT('',#22134);
#5758=VERTEX_POINT('',#22138);
#5759=VERTEX_POINT('',#22142);
#5760=VERTEX_POINT('',#22148);
#5761=VERTEX_POINT('',#22150);
#5762=VERTEX_POINT('',#22154);
#5763=VERTEX_POINT('',#22158);
#5764=VERTEX_POINT('',#22162);
#5765=VERTEX_POINT('',#22166);
#5766=VERTEX_POINT('',#22170);
#5767=VERTEX_POINT('',#22171);
#5768=VERTEX_POINT('',#22176);
#5769=VERTEX_POINT('',#22177);
#5770=VERTEX_POINT('',#22185);
#5771=VERTEX_POINT('',#22186);
#5772=VERTEX_POINT('',#22188);
#5773=VERTEX_POINT('',#22190);
#5774=VERTEX_POINT('',#22192);
#5775=VERTEX_POINT('',#22194);
#5776=VERTEX_POINT('',#22196);
#5777=VERTEX_POINT('',#22198);
#5778=VERTEX_POINT('',#22209);
#5779=VERTEX_POINT('',#22213);
#5780=VERTEX_POINT('',#22234);
#5781=VERTEX_POINT('',#22236);
#5782=VERTEX_POINT('',#22240);
#5783=VERTEX_POINT('',#22241);
#5784=VERTEX_POINT('',#22243);
#5785=VERTEX_POINT('',#22245);
#5786=VERTEX_POINT('',#22248);
#5787=VERTEX_POINT('',#22250);
#5788=VERTEX_POINT('',#22252);
#5789=VERTEX_POINT('',#22254);
#5790=VERTEX_POINT('',#22256);
#5791=VERTEX_POINT('',#22259);
#5792=VERTEX_POINT('',#22263);
#5793=VERTEX_POINT('',#22267);
#5794=VERTEX_POINT('',#22271);
#5795=VERTEX_POINT('',#22275);
#5796=VERTEX_POINT('',#22279);
#5797=VERTEX_POINT('',#22283);
#5798=VERTEX_POINT('',#22287);
#5799=VERTEX_POINT('',#22291);
#5800=VERTEX_POINT('',#22295);
#5801=VERTEX_POINT('',#22299);
#5802=VERTEX_POINT('',#22303);
#5803=VERTEX_POINT('',#22305);
#5804=VERTEX_POINT('',#22309);
#5805=VERTEX_POINT('',#22310);
#5806=VERTEX_POINT('',#22312);
#5807=VERTEX_POINT('',#22314);
#5808=VERTEX_POINT('',#22317);
#5809=VERTEX_POINT('',#22319);
#5810=VERTEX_POINT('',#22321);
#5811=VERTEX_POINT('',#22323);
#5812=VERTEX_POINT('',#22325);
#5813=VERTEX_POINT('',#22327);
#5814=VERTEX_POINT('',#22330);
#5815=VERTEX_POINT('',#22334);
#5816=VERTEX_POINT('',#22336);
#5817=VERTEX_POINT('',#22340);
#5818=VERTEX_POINT('',#22341);
#5819=VERTEX_POINT('',#22346);
#5820=VERTEX_POINT('',#22347);
#5821=VERTEX_POINT('',#22352);
#5822=VERTEX_POINT('',#22353);
#5823=VERTEX_POINT('',#22358);
#5824=VERTEX_POINT('',#22359);
#5825=VERTEX_POINT('',#22364);
#5826=VERTEX_POINT('',#22369);
#5827=VERTEX_POINT('',#22376);
#5828=VERTEX_POINT('',#22382);
#5829=VERTEX_POINT('',#22383);
#5830=VERTEX_POINT('',#22385);
#5831=VERTEX_POINT('',#22387);
#5832=VERTEX_POINT('',#22389);
#5833=VERTEX_POINT('',#22391);
#5834=VERTEX_POINT('',#22393);
#5835=VERTEX_POINT('',#22395);
#5836=VERTEX_POINT('',#22399);
#5837=VERTEX_POINT('',#22403);
#5838=VERTEX_POINT('',#22407);
#5839=VERTEX_POINT('',#22411);
#5840=VERTEX_POINT('',#22415);
#5841=VERTEX_POINT('',#22419);
#5842=VERTEX_POINT('',#22423);
#5843=VERTEX_POINT('',#22427);
#5844=VERTEX_POINT('',#22431);
#5845=VERTEX_POINT('',#22435);
#5846=VERTEX_POINT('',#22439);
#5847=VERTEX_POINT('',#22443);
#5848=VERTEX_POINT('',#22447);
#5849=VERTEX_POINT('',#22451);
#5850=VERTEX_POINT('',#22452);
#5851=VERTEX_POINT('',#22454);
#5852=VERTEX_POINT('',#22456);
#5853=VERTEX_POINT('',#22459);
#5854=VERTEX_POINT('',#22461);
#5855=VERTEX_POINT('',#22463);
#5856=VERTEX_POINT('',#22465);
#5857=VERTEX_POINT('',#22467);
#5858=VERTEX_POINT('',#22469);
#5859=VERTEX_POINT('',#22484);
#5860=VERTEX_POINT('',#22486);
#5861=VERTEX_POINT('',#22490);
#5862=VERTEX_POINT('',#22494);
#5863=VERTEX_POINT('',#22498);
#5864=VERTEX_POINT('',#22502);
#5865=VERTEX_POINT('',#22513);
#5866=VERTEX_POINT('',#22517);
#5867=VERTEX_POINT('',#22521);
#5868=VERTEX_POINT('',#22524);
#5869=VERTEX_POINT('',#22526);
#5870=VERTEX_POINT('',#22528);
#5871=VERTEX_POINT('',#22530);
#5872=VERTEX_POINT('',#22532);
#5873=VERTEX_POINT('',#22534);
#5874=VERTEX_POINT('',#22549);
#5875=VERTEX_POINT('',#22551);
#5876=VERTEX_POINT('',#22555);
#5877=VERTEX_POINT('',#22559);
#5878=VERTEX_POINT('',#22563);
#5879=VERTEX_POINT('',#22564);
#5880=VERTEX_POINT('',#22569);
#5881=VERTEX_POINT('',#22570);
#5882=VERTEX_POINT('',#22575);
#5883=VERTEX_POINT('',#22576);
#5884=VERTEX_POINT('',#22581);
#5885=VERTEX_POINT('',#22590);
#5886=VERTEX_POINT('',#22591);
#5887=VERTEX_POINT('',#22593);
#5888=VERTEX_POINT('',#22595);
#5889=VERTEX_POINT('',#22597);
#5890=VERTEX_POINT('',#22599);
#5891=VERTEX_POINT('',#22601);
#5892=VERTEX_POINT('',#22603);
#5893=VERTEX_POINT('',#22614);
#5894=VERTEX_POINT('',#22618);
#5895=VERTEX_POINT('',#22622);
#5896=VERTEX_POINT('',#22662);
#5897=VERTEX_POINT('',#22663);
#5898=VERTEX_POINT('',#22746);
#5899=VERTEX_POINT('',#22751);
#5900=VERTEX_POINT('',#22841);
#5901=VERTEX_POINT('',#22842);
#5902=VERTEX_POINT('',#22895);
#5903=VERTEX_POINT('',#22900);
#5904=VERTEX_POINT('',#23000);
#5905=VERTEX_POINT('',#23005);
#5906=VERTEX_POINT('',#23012);
#5907=VERTEX_POINT('',#23013);
#5908=VERTEX_POINT('',#23015);
#5909=VERTEX_POINT('',#23017);
#5910=VERTEX_POINT('',#23068);
#5911=VERTEX_POINT('',#23075);
#5912=VERTEX_POINT('',#23108);
#5913=VERTEX_POINT('',#23110);
#5914=VERTEX_POINT('',#23119);
#5915=VERTEX_POINT('',#23121);
#5916=VERTEX_POINT('',#23123);
#5917=VERTEX_POINT('',#23127);
#5918=VERTEX_POINT('',#23129);
#5919=VERTEX_POINT('',#23182);
#5920=VERTEX_POINT('',#23187);
#5921=VERTEX_POINT('',#23192);
#5922=VERTEX_POINT('',#23194);
#5923=VERTEX_POINT('',#23199);
#5924=VERTEX_POINT('',#23276);
#5925=VERTEX_POINT('',#23277);
#5926=VERTEX_POINT('',#23360);
#5927=VERTEX_POINT('',#23365);
#5928=VERTEX_POINT('',#23455);
#5929=VERTEX_POINT('',#23456);
#5930=VERTEX_POINT('',#23509);
#5931=VERTEX_POINT('',#23514);
#5932=VERTEX_POINT('',#23614);
#5933=VERTEX_POINT('',#23619);
#5934=VERTEX_POINT('',#23626);
#5935=VERTEX_POINT('',#23627);
#5936=VERTEX_POINT('',#23629);
#5937=VERTEX_POINT('',#23631);
#5938=VERTEX_POINT('',#23674);
#5939=VERTEX_POINT('',#23679);
#5940=VERTEX_POINT('',#23710);
#5941=VERTEX_POINT('',#23712);
#5942=VERTEX_POINT('',#23714);
#5943=VERTEX_POINT('',#23716);
#5944=VERTEX_POINT('',#23720);
#5945=VERTEX_POINT('',#23729);
#5946=VERTEX_POINT('',#23731);
#5947=VERTEX_POINT('',#23755);
#5948=VERTEX_POINT('',#23756);
#5949=VERTEX_POINT('',#23880);
#5950=VERTEX_POINT('',#23983);
#5951=VERTEX_POINT('',#23990);
#5952=VERTEX_POINT('',#23992);
#5953=VERTEX_POINT('',#24031);
#5954=VERTEX_POINT('',#24058);
#5955=VERTEX_POINT('',#24060);
#5956=VERTEX_POINT('',#24143);
#5957=VERTEX_POINT('',#24151);
#5958=VERTEX_POINT('',#24174);
#5959=VERTEX_POINT('',#24257);
#5960=VERTEX_POINT('',#24350);
#5961=VERTEX_POINT('',#24423);
#5962=VERTEX_POINT('',#24430);
#5963=VERTEX_POINT('',#24431);
#5964=VERTEX_POINT('',#24433);
#5965=VERTEX_POINT('',#24435);
#5966=VERTEX_POINT('',#24478);
#5967=VERTEX_POINT('',#24483);
#5968=VERTEX_POINT('',#24514);
#5969=VERTEX_POINT('',#24516);
#5970=VERTEX_POINT('',#24518);
#5971=VERTEX_POINT('',#24520);
#5972=VERTEX_POINT('',#24533);
#5973=VERTEX_POINT('',#24540);
#5974=VERTEX_POINT('',#24549);
#5975=VERTEX_POINT('',#24558);
#5976=VERTEX_POINT('',#24601);
#5977=VERTEX_POINT('',#24602);
#5978=VERTEX_POINT('',#24649);
#5979=VERTEX_POINT('',#24654);
#5980=VERTEX_POINT('',#24726);
#5981=VERTEX_POINT('',#24727);
#5982=VERTEX_POINT('',#24774);
#5983=VERTEX_POINT('',#24779);
#5984=VERTEX_POINT('',#24851);
#5985=VERTEX_POINT('',#24858);
#5986=VERTEX_POINT('',#24867);
#5987=VERTEX_POINT('',#24869);
#5988=VERTEX_POINT('',#24915);
#5989=VERTEX_POINT('',#24917);
#5990=VERTEX_POINT('',#24919);
#5991=VERTEX_POINT('',#24921);
#5992=VERTEX_POINT('',#24923);
#5993=VERTEX_POINT('',#24925);
#5994=VERTEX_POINT('',#24929);
#5995=VERTEX_POINT('',#24931);
#5996=VERTEX_POINT('',#24985);
#5997=VERTEX_POINT('',#24989);
#5998=VERTEX_POINT('',#24991);
#5999=VERTEX_POINT('',#25068);
#6000=VERTEX_POINT('',#25069);
#6001=VERTEX_POINT('',#25145);
#6002=VERTEX_POINT('',#25220);
#6003=VERTEX_POINT('',#25229);
#6004=VERTEX_POINT('',#25286);
#6005=VERTEX_POINT('',#25333);
#6006=VERTEX_POINT('',#25408);
#6007=VERTEX_POINT('',#25409);
#6008=VERTEX_POINT('',#25456);
#6009=VERTEX_POINT('',#25461);
#6010=VERTEX_POINT('',#25533);
#6011=VERTEX_POINT('',#25540);
#6012=VERTEX_POINT('',#25549);
#6013=VERTEX_POINT('',#25551);
#6014=VERTEX_POINT('',#25591);
#6015=VERTEX_POINT('',#25593);
#6016=VERTEX_POINT('',#25647);
#6017=VERTEX_POINT('',#25651);
#6018=VERTEX_POINT('',#25653);
#6019=VERTEX_POINT('',#25707);
#6020=VERTEX_POINT('',#25735);
#6021=VERTEX_POINT('',#25810);
#6022=VERTEX_POINT('',#25885);
#6023=VERTEX_POINT('',#25894);
#6024=VERTEX_POINT('',#25939);
#6025=VERTEX_POINT('',#25940);
#6026=VERTEX_POINT('',#25944);
#6027=VERTEX_POINT('',#25946);
#6028=VERTEX_POINT('',#25950);
#6029=VERTEX_POINT('',#25952);
#6030=VERTEX_POINT('',#25956);
#6031=VERTEX_POINT('',#25957);
#6032=VERTEX_POINT('',#25964);
#6033=VERTEX_POINT('',#25966);
#6034=VERTEX_POINT('',#25968);
#6035=VERTEX_POINT('',#25970);
#6036=VERTEX_POINT('',#25972);
#6037=VERTEX_POINT('',#25976);
#6038=VERTEX_POINT('',#25979);
#6039=VERTEX_POINT('',#25982);
#6040=VERTEX_POINT('',#25984);
#6041=VERTEX_POINT('',#25986);
#6042=VERTEX_POINT('',#25988);
#6043=VERTEX_POINT('',#25992);
#6044=VERTEX_POINT('',#25994);
#6045=VERTEX_POINT('',#25998);
#6046=VERTEX_POINT('',#25999);
#6047=VERTEX_POINT('',#26001);
#6048=VERTEX_POINT('',#26003);
#6049=VERTEX_POINT('',#26005);
#6050=VERTEX_POINT('',#26007);
#6051=VERTEX_POINT('',#26009);
#6052=VERTEX_POINT('',#26011);
#6053=VERTEX_POINT('',#26015);
#6054=VERTEX_POINT('',#26019);
#6055=VERTEX_POINT('',#26020);
#6056=VERTEX_POINT('',#26024);
#6057=VERTEX_POINT('',#26026);
#6058=VERTEX_POINT('',#26030);
#6059=VERTEX_POINT('',#26032);
#6060=VERTEX_POINT('',#26036);
#6061=VERTEX_POINT('',#26037);
#6062=VERTEX_POINT('',#26044);
#6063=VERTEX_POINT('',#26046);
#6064=VERTEX_POINT('',#26048);
#6065=VERTEX_POINT('',#26050);
#6066=VERTEX_POINT('',#26052);
#6067=VERTEX_POINT('',#26056);
#6068=VERTEX_POINT('',#26059);
#6069=VERTEX_POINT('',#26062);
#6070=VERTEX_POINT('',#26064);
#6071=VERTEX_POINT('',#26066);
#6072=VERTEX_POINT('',#26068);
#6073=VERTEX_POINT('',#26072);
#6074=VERTEX_POINT('',#26074);
#6075=VERTEX_POINT('',#26078);
#6076=VERTEX_POINT('',#26079);
#6077=VERTEX_POINT('',#26084);
#6078=VERTEX_POINT('',#26085);
#6079=VERTEX_POINT('',#26090);
#6080=VERTEX_POINT('',#26091);
#6081=VERTEX_POINT('',#26099);
#6082=VERTEX_POINT('',#26101);
#6083=VERTEX_POINT('',#26103);
#6084=VERTEX_POINT('',#26105);
#6085=VERTEX_POINT('',#26107);
#6086=VERTEX_POINT('',#26109);
#6087=VERTEX_POINT('',#26111);
#6088=VERTEX_POINT('',#26116);
#6089=VERTEX_POINT('',#26120);
#6090=VERTEX_POINT('',#26124);
#6091=VERTEX_POINT('',#26129);
#6092=VERTEX_POINT('',#26131);
#6093=VERTEX_POINT('',#26133);
#6094=VERTEX_POINT('',#26135);
#6095=VERTEX_POINT('',#26137);
#6096=VERTEX_POINT('',#26139);
#6097=VERTEX_POINT('',#26143);
#6098=VERTEX_POINT('',#26147);
#6099=VERTEX_POINT('',#26148);
#6100=VERTEX_POINT('',#26153);
#6101=VERTEX_POINT('',#26154);
#6102=VERTEX_POINT('',#26159);
#6103=VERTEX_POINT('',#26166);
#6104=VERTEX_POINT('',#26170);
#6105=VERTEX_POINT('',#26177);
#6106=VERTEX_POINT('',#26191);
#6107=VERTEX_POINT('',#26197);
#6108=VERTEX_POINT('',#26201);
#6109=VERTEX_POINT('',#26203);
#6110=VERTEX_POINT('',#26207);
#6111=VERTEX_POINT('',#26209);
#6112=VERTEX_POINT('',#26216);
#6113=VERTEX_POINT('',#26218);
#6114=VERTEX_POINT('',#26222);
#6115=VERTEX_POINT('',#26226);
#6116=VERTEX_POINT('',#26230);
#6117=VERTEX_POINT('',#26235);
#6118=VERTEX_POINT('',#26239);
#6119=VERTEX_POINT('',#26243);
#6120=VERTEX_POINT('',#26252);
#6121=VERTEX_POINT('',#26253);
#6122=VERTEX_POINT('',#26255);
#6123=VERTEX_POINT('',#26257);
#6124=VERTEX_POINT('',#26260);
#6125=VERTEX_POINT('',#26261);
#6126=VERTEX_POINT('',#26263);
#6127=VERTEX_POINT('',#26265);
#6128=VERTEX_POINT('',#26268);
#6129=VERTEX_POINT('',#26269);
#6130=VERTEX_POINT('',#26271);
#6131=VERTEX_POINT('',#26273);
#6132=VERTEX_POINT('',#26276);
#6133=VERTEX_POINT('',#26277);
#6134=VERTEX_POINT('',#26279);
#6135=VERTEX_POINT('',#26281);
#6136=VERTEX_POINT('',#26285);
#6137=VERTEX_POINT('',#26289);
#6138=VERTEX_POINT('',#26290);
#6139=VERTEX_POINT('',#26295);
#6140=VERTEX_POINT('',#26300);
#6141=VERTEX_POINT('',#26307);
#6142=VERTEX_POINT('',#26311);
#6143=VERTEX_POINT('',#26315);
#6144=VERTEX_POINT('',#26319);
#6145=VERTEX_POINT('',#26326);
#6146=VERTEX_POINT('',#26328);
#6147=VERTEX_POINT('',#26332);
#6148=VERTEX_POINT('',#26334);
#6149=VERTEX_POINT('',#26342);
#6150=VERTEX_POINT('',#26344);
#6151=VERTEX_POINT('',#26348);
#6152=VERTEX_POINT('',#26351);
#6153=VERTEX_POINT('',#26354);
#6154=VERTEX_POINT('',#26356);
#6155=VERTEX_POINT('',#26360);
#6156=VERTEX_POINT('',#26362);
#6157=VERTEX_POINT('',#26370);
#6158=VERTEX_POINT('',#26372);
#6159=VERTEX_POINT('',#26376);
#6160=VERTEX_POINT('',#26379);
#6161=VERTEX_POINT('',#26382);
#6162=VERTEX_POINT('',#26384);
#6163=VERTEX_POINT('',#26388);
#6164=VERTEX_POINT('',#26390);
#6165=VERTEX_POINT('',#26398);
#6166=VERTEX_POINT('',#26400);
#6167=VERTEX_POINT('',#26404);
#6168=VERTEX_POINT('',#26407);
#6169=VERTEX_POINT('',#26410);
#6170=VERTEX_POINT('',#26412);
#6171=VERTEX_POINT('',#26416);
#6172=VERTEX_POINT('',#26418);
#6173=VERTEX_POINT('',#26426);
#6174=VERTEX_POINT('',#26428);
#6175=VERTEX_POINT('',#26432);
#6176=VERTEX_POINT('',#26435);
#6177=VERTEX_POINT('',#26438);
#6178=VERTEX_POINT('',#26442);
#6179=VERTEX_POINT('',#26446);
#6180=VERTEX_POINT('',#26450);
#6181=VERTEX_POINT('',#26456);
#6182=VERTEX_POINT('',#26463);
#6183=VERTEX_POINT('',#26470);
#6184=VERTEX_POINT('',#26477);
#6185=VERTEX_POINT('',#26495);
#6186=VERTEX_POINT('',#26497);
#6187=VERTEX_POINT('',#26499);
#6188=VERTEX_POINT('',#26503);
#6189=VERTEX_POINT('',#26505);
#6190=VERTEX_POINT('',#26510);
#6191=VERTEX_POINT('',#26512);
#6192=VERTEX_POINT('',#26516);
#6193=VERTEX_POINT('',#26520);
#6194=VERTEX_POINT('',#26526);
#6195=VERTEX_POINT('',#26529);
#6196=VERTEX_POINT('',#26533);
#6197=VERTEX_POINT('',#26537);
#6198=VERTEX_POINT('',#26543);
#6199=VERTEX_POINT('',#26544);
#6200=VERTEX_POINT('',#26546);
#6201=VERTEX_POINT('',#26548);
#6202=VERTEX_POINT('',#26552);
#6203=VERTEX_POINT('',#26554);
#6204=VERTEX_POINT('',#26558);
#6205=VERTEX_POINT('',#26560);
#6206=VERTEX_POINT('',#26564);
#6207=VERTEX_POINT('',#26566);
#6208=VERTEX_POINT('',#26570);
#6209=VERTEX_POINT('',#26572);
#6210=VERTEX_POINT('',#26576);
#6211=VERTEX_POINT('',#26578);
#6212=VERTEX_POINT('',#26582);
#6213=VERTEX_POINT('',#26584);
#6214=VERTEX_POINT('',#26588);
#6215=VERTEX_POINT('',#26590);
#6216=VERTEX_POINT('',#26594);
#6217=VERTEX_POINT('',#26596);
#6218=VERTEX_POINT('',#26600);
#6219=VERTEX_POINT('',#26602);
#6220=VERTEX_POINT('',#26606);
#6221=VERTEX_POINT('',#26608);
#6222=VERTEX_POINT('',#26612);
#6223=VERTEX_POINT('',#26614);
#6224=VERTEX_POINT('',#26618);
#6225=VERTEX_POINT('',#26620);
#6226=VERTEX_POINT('',#26624);
#6227=VERTEX_POINT('',#26626);
#6228=VERTEX_POINT('',#26630);
#6229=VERTEX_POINT('',#26632);
#6230=VERTEX_POINT('',#26636);
#6231=VERTEX_POINT('',#26638);
#6232=VERTEX_POINT('',#26642);
#6233=VERTEX_POINT('',#26644);
#6234=VERTEX_POINT('',#26648);
#6235=VERTEX_POINT('',#26650);
#6236=VERTEX_POINT('',#26654);
#6237=VERTEX_POINT('',#26656);
#6238=VERTEX_POINT('',#26660);
#6239=VERTEX_POINT('',#26662);
#6240=VERTEX_POINT('',#26666);
#6241=VERTEX_POINT('',#26668);
#6242=VERTEX_POINT('',#26672);
#6243=VERTEX_POINT('',#26674);
#6244=VERTEX_POINT('',#26678);
#6245=VERTEX_POINT('',#26680);
#6246=VERTEX_POINT('',#26684);
#6247=VERTEX_POINT('',#26686);
#6248=VERTEX_POINT('',#26690);
#6249=VERTEX_POINT('',#26692);
#6250=VERTEX_POINT('',#26696);
#6251=VERTEX_POINT('',#26698);
#6252=VERTEX_POINT('',#26702);
#6253=VERTEX_POINT('',#26704);
#6254=VERTEX_POINT('',#26708);
#6255=VERTEX_POINT('',#26710);
#6256=VERTEX_POINT('',#26714);
#6257=VERTEX_POINT('',#26716);
#6258=VERTEX_POINT('',#26720);
#6259=VERTEX_POINT('',#26722);
#6260=VERTEX_POINT('',#26726);
#6261=VERTEX_POINT('',#26728);
#6262=VERTEX_POINT('',#26732);
#6263=VERTEX_POINT('',#26734);
#6264=VERTEX_POINT('',#26738);
#6265=VERTEX_POINT('',#26740);
#6266=VERTEX_POINT('',#26744);
#6267=VERTEX_POINT('',#26746);
#6268=VERTEX_POINT('',#26750);
#6269=VERTEX_POINT('',#26752);
#6270=VERTEX_POINT('',#26756);
#6271=VERTEX_POINT('',#26758);
#6272=VERTEX_POINT('',#26762);
#6273=VERTEX_POINT('',#26764);
#6274=VERTEX_POINT('',#26768);
#6275=VERTEX_POINT('',#26770);
#6276=VERTEX_POINT('',#26774);
#6277=VERTEX_POINT('',#26776);
#6278=VERTEX_POINT('',#26780);
#6279=VERTEX_POINT('',#26782);
#6280=VERTEX_POINT('',#26786);
#6281=VERTEX_POINT('',#26788);
#6282=VERTEX_POINT('',#26792);
#6283=VERTEX_POINT('',#26794);
#6284=VERTEX_POINT('',#26798);
#6285=VERTEX_POINT('',#26800);
#6286=VERTEX_POINT('',#26804);
#6287=VERTEX_POINT('',#26806);
#6288=VERTEX_POINT('',#26810);
#6289=VERTEX_POINT('',#26812);
#6290=VERTEX_POINT('',#26816);
#6291=VERTEX_POINT('',#26818);
#6292=VERTEX_POINT('',#26822);
#6293=VERTEX_POINT('',#26824);
#6294=VERTEX_POINT('',#26828);
#6295=VERTEX_POINT('',#26830);
#6296=VERTEX_POINT('',#26834);
#6297=VERTEX_POINT('',#26836);
#6298=VERTEX_POINT('',#26846);
#6299=VERTEX_POINT('',#26847);
#6300=VERTEX_POINT('',#26849);
#6301=VERTEX_POINT('',#26851);
#6302=VERTEX_POINT('',#26855);
#6303=VERTEX_POINT('',#26856);
#6304=VERTEX_POINT('',#26861);
#6305=VERTEX_POINT('',#26862);
#6306=VERTEX_POINT('',#26867);
#6307=VERTEX_POINT('',#26868);
#6308=VERTEX_POINT('',#26873);
#6309=VERTEX_POINT('',#26874);
#6310=VERTEX_POINT('',#26879);
#6311=VERTEX_POINT('',#26880);
#6312=VERTEX_POINT('',#26885);
#6313=VERTEX_POINT('',#26886);
#6314=VERTEX_POINT('',#26894);
#6315=VERTEX_POINT('',#26896);
#6316=VERTEX_POINT('',#26900);
#6317=VERTEX_POINT('',#26904);
#6318=VERTEX_POINT('',#26908);
#6319=VERTEX_POINT('',#26912);
#6320=VERTEX_POINT('',#26913);
#6321=VERTEX_POINT('',#26915);
#6322=VERTEX_POINT('',#26917);
#6323=VERTEX_POINT('',#26919);
#6324=VERTEX_POINT('',#26921);
#6325=VERTEX_POINT('',#26923);
#6326=VERTEX_POINT('',#26925);
#6327=VERTEX_POINT('',#26929);
#6328=VERTEX_POINT('',#26930);
#6329=VERTEX_POINT('',#26932);
#6330=VERTEX_POINT('',#26934);
#6331=VERTEX_POINT('',#26938);
#6332=VERTEX_POINT('',#26939);
#6333=VERTEX_POINT('',#26944);
#6334=VERTEX_POINT('',#26945);
#6335=VERTEX_POINT('',#26950);
#6336=VERTEX_POINT('',#26951);
#6337=VERTEX_POINT('',#26956);
#6338=VERTEX_POINT('',#26957);
#6339=VERTEX_POINT('',#26962);
#6340=VERTEX_POINT('',#26963);
#6341=VERTEX_POINT('',#26968);
#6342=VERTEX_POINT('',#26969);
#6343=VERTEX_POINT('',#26986);
#6344=VERTEX_POINT('',#26987);
#6345=VERTEX_POINT('',#26989);
#6346=VERTEX_POINT('',#26991);
#6347=VERTEX_POINT('',#26993);
#6348=VERTEX_POINT('',#26995);
#6349=VERTEX_POINT('',#26997);
#6350=VERTEX_POINT('',#26999);
#6351=VERTEX_POINT('',#27003);
#6352=VERTEX_POINT('',#27005);
#6353=VERTEX_POINT('',#27009);
#6354=VERTEX_POINT('',#27013);
#6355=VERTEX_POINT('',#27017);
#6356=VERTEX_POINT('',#27021);
#6357=VERTEX_POINT('',#27025);
#6358=VERTEX_POINT('',#27029);
#6359=VERTEX_POINT('',#27035);
#6360=VERTEX_POINT('',#27037);
#6361=VERTEX_POINT('',#27039);
#6362=VERTEX_POINT('',#27041);
#6363=VERTEX_POINT('',#27045);
#6364=VERTEX_POINT('',#27047);
#6365=VERTEX_POINT('',#27115);
#6366=VERTEX_POINT('',#27121);
#6367=VERTEX_POINT('',#27126);
#6368=VERTEX_POINT('',#27128);
#6369=VERTEX_POINT('',#27133);
#6370=VERTEX_POINT('',#27209);
#6371=VERTEX_POINT('',#27211);
#6372=VERTEX_POINT('',#27213);
#6373=VERTEX_POINT('',#27217);
#6374=VERTEX_POINT('',#27219);
#6375=VERTEX_POINT('',#27287);
#6376=VERTEX_POINT('',#27294);
#6377=VERTEX_POINT('',#27299);
#6378=VERTEX_POINT('',#27301);
#6379=VERTEX_POINT('',#27306);
#6380=VERTEX_POINT('',#27419);
#6381=VERTEX_POINT('',#27517);
#6382=VERTEX_POINT('',#27629);
#6383=VERTEX_POINT('',#27630);
#6384=VERTEX_POINT('',#27698);
#6385=VERTEX_POINT('',#27703);
#6386=VERTEX_POINT('',#27822);
#6387=VERTEX_POINT('',#27828);
#6388=VERTEX_POINT('',#27836);
#6389=VERTEX_POINT('',#27837);
#6390=VERTEX_POINT('',#27839);
#6391=VERTEX_POINT('',#27841);
#6392=VERTEX_POINT('',#27900);
#6393=VERTEX_POINT('',#27909);
#6394=VERTEX_POINT('',#27944);
#6395=VERTEX_POINT('',#28042);
#6396=VERTEX_POINT('',#28093);
#6397=VERTEX_POINT('',#28094);
#6398=VERTEX_POINT('',#28192);
#6399=VERTEX_POINT('',#28197);
#6400=VERTEX_POINT('',#28306);
#6401=VERTEX_POINT('',#28307);
#6402=VERTEX_POINT('',#28375);
#6403=VERTEX_POINT('',#28380);
#6404=VERTEX_POINT('',#28511);
#6405=VERTEX_POINT('',#28520);
#6406=VERTEX_POINT('',#28531);
#6407=VERTEX_POINT('',#28532);
#6408=VERTEX_POINT('',#28534);
#6409=VERTEX_POINT('',#28536);
#6410=VERTEX_POINT('',#28583);
#6411=VERTEX_POINT('',#28589);
#6412=VERTEX_POINT('',#28628);
#6413=VERTEX_POINT('',#28630);
#6414=VERTEX_POINT('',#28634);
#6415=VERTEX_POINT('',#28638);
#6416=VERTEX_POINT('',#28642);
#6417=VERTEX_POINT('',#28646);
#6418=VERTEX_POINT('',#28647);
#6419=VERTEX_POINT('',#28652);
#6420=VERTEX_POINT('',#28653);
#6421=VERTEX_POINT('',#28658);
#6422=VERTEX_POINT('',#28659);
#6423=VERTEX_POINT('',#28667);
#6424=VERTEX_POINT('',#28672);
#6425=VERTEX_POINT('',#28674);
#6426=VERTEX_POINT('',#28679);
#6427=VERTEX_POINT('',#28681);
#6428=VERTEX_POINT('',#28686);
#6429=VERTEX_POINT('',#28688);
#6430=VERTEX_POINT('',#28734);
#6431=VERTEX_POINT('',#28971);
#6432=VERTEX_POINT('',#29114);
#6433=VERTEX_POINT('',#29115);
#6434=VERTEX_POINT('',#29368);
#6435=VERTEX_POINT('',#29369);
#6436=VERTEX_POINT('',#29371);
#6437=VERTEX_POINT('',#29373);
#6438=VERTEX_POINT('',#29375);
#6439=VERTEX_POINT('',#29377);
#6440=VERTEX_POINT('',#29381);
#6441=VERTEX_POINT('',#29382);
#6442=VERTEX_POINT('',#29387);
#6443=VERTEX_POINT('',#29388);
#6444=VERTEX_POINT('',#29393);
#6445=VERTEX_POINT('',#29394);
#6446=VERTEX_POINT('',#29399);
#6447=VERTEX_POINT('',#29400);
#6448=VERTEX_POINT('',#29405);
#6449=VERTEX_POINT('',#29406);
#6450=VERTEX_POINT('',#29411);
#6451=VERTEX_POINT('',#29412);
#6452=VERTEX_POINT('',#29420);
#6453=VERTEX_POINT('',#29422);
#6454=VERTEX_POINT('',#29424);
#6455=VERTEX_POINT('',#29426);
#6456=VERTEX_POINT('',#29428);
#6457=VERTEX_POINT('',#29430);
#6458=VERTEX_POINT('',#29432);
#6459=VERTEX_POINT('',#29434);
#6460=VERTEX_POINT('',#29436);
#6461=VERTEX_POINT('',#29438);
#6462=VERTEX_POINT('',#29440);
#6463=VERTEX_POINT('',#29442);
#6464=VERTEX_POINT('',#29446);
#6465=VERTEX_POINT('',#29448);
#6466=VERTEX_POINT('',#29452);
#6467=VERTEX_POINT('',#29456);
#6468=VERTEX_POINT('',#29460);
#6469=VERTEX_POINT('',#29464);
#6470=VERTEX_POINT('',#29465);
#6471=VERTEX_POINT('',#29467);
#6472=VERTEX_POINT('',#29471);
#6473=VERTEX_POINT('',#29472);
#6474=VERTEX_POINT('',#29475);
#6475=VERTEX_POINT('',#29479);
#6476=VERTEX_POINT('',#29480);
#6477=VERTEX_POINT('',#29483);
#6478=VERTEX_POINT('',#29490);
#6479=VERTEX_POINT('',#29494);
#6480=VERTEX_POINT('',#29496);
#6481=VERTEX_POINT('',#29535);
#6482=VERTEX_POINT('',#29536);
#6483=VERTEX_POINT('',#29631);
#6484=VERTEX_POINT('',#29636);
#6485=VERTEX_POINT('',#29740);
#6486=VERTEX_POINT('',#29741);
#6487=VERTEX_POINT('',#29812);
#6488=VERTEX_POINT('',#29817);
#6489=VERTEX_POINT('',#29933);
#6490=VERTEX_POINT('',#29939);
#6491=VERTEX_POINT('',#29947);
#6492=VERTEX_POINT('',#29948);
#6493=VERTEX_POINT('',#29950);
#6494=VERTEX_POINT('',#29952);
#6495=VERTEX_POINT('',#29999);
#6496=VERTEX_POINT('',#30005);
#6497=VERTEX_POINT('',#30037);
#6498=VERTEX_POINT('',#30039);
#6499=VERTEX_POINT('',#30134);
#6500=VERTEX_POINT('',#30142);
#6501=VERTEX_POINT('',#30144);
#6502=VERTEX_POINT('',#30146);
#6503=VERTEX_POINT('',#30150);
#6504=VERTEX_POINT('',#30193);
#6505=VERTEX_POINT('',#30194);
#6506=VERTEX_POINT('',#30289);
#6507=VERTEX_POINT('',#30294);
#6508=VERTEX_POINT('',#30398);
#6509=VERTEX_POINT('',#30493);
#6510=VERTEX_POINT('',#30501);
#6511=VERTEX_POINT('',#30502);
#6512=VERTEX_POINT('',#30504);
#6513=VERTEX_POINT('',#30506);
#6514=VERTEX_POINT('',#30553);
#6515=VERTEX_POINT('',#30559);
#6516=VERTEX_POINT('',#30591);
#6517=VERTEX_POINT('',#30593);
#6518=VERTEX_POINT('',#30598);
#6519=VERTEX_POINT('',#30600);
#6520=VERTEX_POINT('',#30605);
#6521=VERTEX_POINT('',#30607);
#6522=VERTEX_POINT('',#30612);
#6523=VERTEX_POINT('',#30614);
#6524=VERTEX_POINT('',#30621);
#6525=VERTEX_POINT('',#30625);
#6526=VERTEX_POINT('',#30629);
#6527=VERTEX_POINT('',#30630);
#6528=VERTEX_POINT('',#30635);
#6529=VERTEX_POINT('',#30639);
#6530=VERTEX_POINT('',#30650);
#6531=VERTEX_POINT('',#30654);
#6532=VERTEX_POINT('',#30658);
#6533=VERTEX_POINT('',#30670);
#6534=VERTEX_POINT('',#30672);
#6535=VERTEX_POINT('',#30676);
#6536=VERTEX_POINT('',#30678);
#6537=VERTEX_POINT('',#30749);
#6538=VERTEX_POINT('',#30755);
#6539=VERTEX_POINT('',#30760);
#6540=VERTEX_POINT('',#30762);
#6541=VERTEX_POINT('',#30767);
#6542=VERTEX_POINT('',#30892);
#6543=VERTEX_POINT('',#30893);
#6544=VERTEX_POINT('',#30988);
#6545=VERTEX_POINT('',#30993);
#6546=VERTEX_POINT('',#31097);
#6547=VERTEX_POINT('',#31098);
#6548=VERTEX_POINT('',#31169);
#6549=VERTEX_POINT('',#31174);
#6550=VERTEX_POINT('',#31290);
#6551=VERTEX_POINT('',#31303);
#6552=VERTEX_POINT('',#31305);
#6553=VERTEX_POINT('',#31353);
#6554=VERTEX_POINT('',#31426);
#6555=VERTEX_POINT('',#31427);
#6556=VERTEX_POINT('',#31559);
#6557=VERTEX_POINT('',#31750);
#6558=VERTEX_POINT('',#31754);
#6559=VERTEX_POINT('',#31758);
#6560=VERTEX_POINT('',#31766);
#6561=VERTEX_POINT('',#31768);
#6562=VERTEX_POINT('',#31772);
#6563=VERTEX_POINT('',#31776);
#6564=VERTEX_POINT('',#31777);
#6565=VERTEX_POINT('',#31779);
#6566=VERTEX_POINT('',#31781);
#6567=VERTEX_POINT('',#31783);
#6568=VERTEX_POINT('',#31785);
#6569=VERTEX_POINT('',#31787);
#6570=VERTEX_POINT('',#31789);
#6571=VERTEX_POINT('',#31791);
#6572=VERTEX_POINT('',#31793);
#6573=VERTEX_POINT('',#31797);
#6574=VERTEX_POINT('',#31801);
#6575=VERTEX_POINT('',#31802);
#6576=VERTEX_POINT('',#31804);
#6577=VERTEX_POINT('',#31806);
#6578=VERTEX_POINT('',#31808);
#6579=VERTEX_POINT('',#31810);
#6580=VERTEX_POINT('',#31812);
#6581=VERTEX_POINT('',#31814);
#6582=VERTEX_POINT('',#31816);
#6583=VERTEX_POINT('',#31818);
#6584=VERTEX_POINT('',#31820);
#6585=VERTEX_POINT('',#31822);
#6586=VERTEX_POINT('',#31824);
#6587=VERTEX_POINT('',#31826);
#6588=VERTEX_POINT('',#31828);
#6589=VERTEX_POINT('',#31830);
#6590=VERTEX_POINT('',#31832);
#6591=VERTEX_POINT('',#31834);
#6592=VERTEX_POINT('',#31836);
#6593=VERTEX_POINT('',#31838);
#6594=VERTEX_POINT('',#31840);
#6595=VERTEX_POINT('',#31842);
#6596=VERTEX_POINT('',#31844);
#6597=VERTEX_POINT('',#31846);
#6598=VERTEX_POINT('',#31848);
#6599=VERTEX_POINT('',#31850);
#6600=VERTEX_POINT('',#31852);
#6601=VERTEX_POINT('',#31854);
#6602=VERTEX_POINT('',#31856);
#6603=VERTEX_POINT('',#31858);
#6604=VERTEX_POINT('',#31860);
#6605=VERTEX_POINT('',#31862);
#6606=VERTEX_POINT('',#31864);
#6607=VERTEX_POINT('',#31866);
#6608=VERTEX_POINT('',#31868);
#6609=VERTEX_POINT('',#31870);
#6610=VERTEX_POINT('',#31872);
#6611=VERTEX_POINT('',#31874);
#6612=VERTEX_POINT('',#31876);
#6613=VERTEX_POINT('',#31878);
#6614=VERTEX_POINT('',#31880);
#6615=VERTEX_POINT('',#31882);
#6616=VERTEX_POINT('',#31884);
#6617=VERTEX_POINT('',#31886);
#6618=VERTEX_POINT('',#31888);
#6619=VERTEX_POINT('',#31890);
#6620=VERTEX_POINT('',#31892);
#6621=VERTEX_POINT('',#31894);
#6622=VERTEX_POINT('',#31896);
#6623=VERTEX_POINT('',#31898);
#6624=VERTEX_POINT('',#31900);
#6625=VERTEX_POINT('',#31902);
#6626=VERTEX_POINT('',#31904);
#6627=VERTEX_POINT('',#31906);
#6628=VERTEX_POINT('',#31908);
#6629=VERTEX_POINT('',#31910);
#6630=VERTEX_POINT('',#31912);
#6631=VERTEX_POINT('',#31914);
#6632=VERTEX_POINT('',#31916);
#6633=VERTEX_POINT('',#31918);
#6634=VERTEX_POINT('',#31922);
#6635=VERTEX_POINT('',#31924);
#6636=VERTEX_POINT('',#31928);
#6637=VERTEX_POINT('',#31930);
#6638=VERTEX_POINT('',#31934);
#6639=VERTEX_POINT('',#31936);
#6640=VERTEX_POINT('',#31940);
#6641=VERTEX_POINT('',#31942);
#6642=VERTEX_POINT('',#31946);
#6643=VERTEX_POINT('',#31948);
#6644=VERTEX_POINT('',#31952);
#6645=VERTEX_POINT('',#31954);
#6646=VERTEX_POINT('',#31958);
#6647=VERTEX_POINT('',#31959);
#6648=VERTEX_POINT('',#31964);
#6649=VERTEX_POINT('',#31966);
#6650=VERTEX_POINT('',#31970);
#6651=VERTEX_POINT('',#31971);
#6652=VERTEX_POINT('',#31978);
#6653=VERTEX_POINT('',#31979);
#6654=VERTEX_POINT('',#31986);
#6655=VERTEX_POINT('',#31987);
#6656=VERTEX_POINT('',#32001);
#6657=VERTEX_POINT('',#32003);
#6658=VERTEX_POINT('',#32007);
#6659=VERTEX_POINT('',#32009);
#6660=VERTEX_POINT('',#32014);
#6661=VERTEX_POINT('',#32016);
#6662=VERTEX_POINT('',#32020);
#6663=VERTEX_POINT('',#32024);
#6664=VERTEX_POINT('',#32028);
#6665=VERTEX_POINT('',#32030);
#6666=VERTEX_POINT('',#32034);
#6667=VERTEX_POINT('',#32036);
#6668=VERTEX_POINT('',#32040);
#6669=VERTEX_POINT('',#32042);
#6670=VERTEX_POINT('',#32046);
#6671=VERTEX_POINT('',#32048);
#6672=VERTEX_POINT('',#32052);
#6673=VERTEX_POINT('',#32054);
#6674=VERTEX_POINT('',#32058);
#6675=VERTEX_POINT('',#32060);
#6676=VERTEX_POINT('',#32064);
#6677=VERTEX_POINT('',#32066);
#6678=VERTEX_POINT('',#32070);
#6679=VERTEX_POINT('',#32072);
#6680=VERTEX_POINT('',#32076);
#6681=VERTEX_POINT('',#32078);
#6682=VERTEX_POINT('',#32082);
#6683=VERTEX_POINT('',#32084);
#6684=VERTEX_POINT('',#32088);
#6685=VERTEX_POINT('',#32090);
#6686=VERTEX_POINT('',#32094);
#6687=VERTEX_POINT('',#32096);
#6688=VERTEX_POINT('',#32100);
#6689=VERTEX_POINT('',#32104);
#6690=VERTEX_POINT('',#32105);
#6691=VERTEX_POINT('',#32112);
#6692=VERTEX_POINT('',#32113);
#6693=VERTEX_POINT('',#32120);
#6694=VERTEX_POINT('',#32121);
#6695=VERTEX_POINT('',#32128);
#6696=VERTEX_POINT('',#32130);
#6697=VERTEX_POINT('',#32134);
#6698=VERTEX_POINT('',#32158);
#6699=VERTEX_POINT('',#32160);
#6700=VERTEX_POINT('',#32164);
#6701=VERTEX_POINT('',#32166);
#6702=VERTEX_POINT('',#32170);
#6703=VERTEX_POINT('',#32172);
#6704=VERTEX_POINT('',#32176);
#6705=VERTEX_POINT('',#32178);
#6706=VERTEX_POINT('',#32182);
#6707=VERTEX_POINT('',#32184);
#6708=VERTEX_POINT('',#32188);
#6709=VERTEX_POINT('',#32190);
#6710=VERTEX_POINT('',#32194);
#6711=VERTEX_POINT('',#32196);
#6712=VERTEX_POINT('',#32200);
#6713=VERTEX_POINT('',#32201);
#6714=VERTEX_POINT('',#32251);
#6715=VERTEX_POINT('',#32255);
#6716=EDGE_CURVE('',#5518,#5519,#2896,.T.);
#6717=EDGE_CURVE('',#5519,#5520,#2897,.T.);
#6718=EDGE_CURVE('',#5520,#5521,#2898,.T.);
#6719=EDGE_CURVE('',#5521,#5518,#2899,.T.);
#6720=EDGE_CURVE('',#5522,#5523,#2900,.T.);
#6721=EDGE_CURVE('',#5523,#5519,#773,.T.);
#6722=EDGE_CURVE('',#5518,#5522,#774,.T.);
#6723=EDGE_CURVE('',#5524,#5525,#2901,.T.);
#6724=EDGE_CURVE('',#5525,#5523,#2902,.T.);
#6725=EDGE_CURVE('',#5522,#5524,#2903,.T.);
#6726=EDGE_CURVE('',#5526,#5527,#2904,.T.);
#6727=EDGE_CURVE('',#5527,#5525,#775,.T.);
#6728=EDGE_CURVE('',#5524,#5526,#776,.T.);
#6729=EDGE_CURVE('',#5528,#5529,#2905,.T.);
#6730=EDGE_CURVE('',#5529,#5527,#2906,.T.);
#6731=EDGE_CURVE('',#5526,#5528,#2907,.T.);
#6732=EDGE_CURVE('',#5530,#5531,#2908,.T.);
#6733=EDGE_CURVE('',#5531,#5529,#777,.T.);
#6734=EDGE_CURVE('',#5528,#5530,#778,.T.);
#6735=EDGE_CURVE('',#5532,#5533,#2909,.T.);
#6736=EDGE_CURVE('',#5533,#5531,#2910,.T.);
#6737=EDGE_CURVE('',#5530,#5532,#2911,.T.);
#6738=EDGE_CURVE('',#5520,#5533,#779,.T.);
#6739=EDGE_CURVE('',#5532,#5521,#780,.T.);
#6740=EDGE_CURVE('',#5534,#5524,#2912,.T.);
#6741=EDGE_CURVE('',#5535,#5534,#781,.T.);
#6742=EDGE_CURVE('',#5535,#5526,#2913,.T.);
#6743=EDGE_CURVE('',#5536,#5522,#2914,.T.);
#6744=EDGE_CURVE('',#5534,#5536,#2915,.T.);
#6745=EDGE_CURVE('',#5537,#5537,#782,.T.);
#6746=EDGE_CURVE('',#5538,#5518,#2916,.T.);
#6747=EDGE_CURVE('',#5536,#5538,#783,.T.);
#6748=EDGE_CURVE('',#5539,#5521,#2917,.T.);
#6749=EDGE_CURVE('',#5538,#5539,#2918,.T.);
#6750=EDGE_CURVE('',#5540,#5541,#2919,.T.);
#6751=EDGE_CURVE('',#5542,#5540,#784,.T.);
#6752=EDGE_CURVE('',#5543,#5542,#2920,.T.);
#6753=EDGE_CURVE('',#5544,#5543,#785,.T.);
#6754=EDGE_CURVE('',#5545,#5544,#2921,.T.);
#6755=EDGE_CURVE('',#5546,#5545,#786,.T.);
#6756=EDGE_CURVE('',#5547,#5546,#2922,.T.);
#6757=EDGE_CURVE('',#5541,#5547,#787,.T.);
#6758=EDGE_CURVE('',#5548,#5540,#2923,.T.);
#6759=EDGE_CURVE('',#5541,#5549,#2924,.T.);
#6760=EDGE_CURVE('',#5549,#5548,#2925,.T.);
#6761=EDGE_CURVE('',#5550,#5542,#2926,.T.);
#6762=EDGE_CURVE('',#5548,#5550,#788,.T.);
#6763=EDGE_CURVE('',#5551,#5543,#2927,.T.);
#6764=EDGE_CURVE('',#5550,#5551,#2928,.T.);
#6765=EDGE_CURVE('',#5552,#5544,#2929,.T.);
#6766=EDGE_CURVE('',#5551,#5552,#789,.T.);
#6767=EDGE_CURVE('',#5553,#5545,#2930,.T.);
#6768=EDGE_CURVE('',#5552,#5553,#2931,.T.);
#6769=EDGE_CURVE('',#5554,#5546,#2932,.T.);
#6770=EDGE_CURVE('',#5553,#5554,#790,.T.);
#6771=EDGE_CURVE('',#5555,#5547,#2933,.T.);
#6772=EDGE_CURVE('',#5554,#5555,#2934,.T.);
#6773=EDGE_CURVE('',#5555,#5549,#791,.T.);
#6774=EDGE_CURVE('',#5556,#5551,#2935,.T.);
#6775=EDGE_CURVE('',#5557,#5556,#792,.T.);
#6776=EDGE_CURVE('',#5557,#5552,#2936,.T.);
#6777=EDGE_CURVE('',#5558,#5550,#2937,.T.);
#6778=EDGE_CURVE('',#5556,#5558,#2938,.T.);
#6779=EDGE_CURVE('',#5559,#5548,#2939,.T.);
#6780=EDGE_CURVE('',#5558,#5559,#793,.T.);
#6781=EDGE_CURVE('',#5560,#5549,#2940,.T.);
#6782=EDGE_CURVE('',#5559,#5560,#2941,.T.);
#6783=EDGE_CURVE('',#5561,#5556,#2942,.T.);
#6784=EDGE_CURVE('',#5558,#5562,#2943,.T.);
#6785=EDGE_CURVE('',#5562,#5561,#2944,.T.);
#6786=EDGE_CURVE('',#5563,#5557,#2945,.T.);
#6787=EDGE_CURVE('',#5561,#5563,#794,.T.);
#6788=EDGE_CURVE('',#5564,#5565,#2946,.T.);
#6789=EDGE_CURVE('',#5565,#5557,#2947,.T.);
#6790=EDGE_CURVE('',#5563,#5564,#2948,.T.);
#6791=EDGE_CURVE('',#5566,#5567,#2949,.T.);
#6792=EDGE_CURVE('',#5567,#5565,#795,.T.);
#6793=EDGE_CURVE('',#5564,#5566,#796,.T.);
#6794=EDGE_CURVE('',#5568,#5569,#2950,.T.);
#6795=EDGE_CURVE('',#5569,#5567,#2951,.T.);
#6796=EDGE_CURVE('',#5566,#5568,#2952,.T.);
#6797=EDGE_CURVE('',#5570,#5560,#2953,.T.);
#6798=EDGE_CURVE('',#5560,#5569,#797,.T.);
#6799=EDGE_CURVE('',#5568,#5570,#798,.T.);
#6800=EDGE_CURVE('',#5571,#5559,#2954,.T.);
#6801=EDGE_CURVE('',#5570,#5571,#2955,.T.);
#6802=EDGE_CURVE('',#5571,#5562,#799,.T.);
#6803=EDGE_CURVE('',#5569,#5555,#2956,.T.);
#6804=EDGE_CURVE('',#5572,#5573,#2957,.T.);
#6805=EDGE_CURVE('',#5574,#5572,#800,.T.);
#6806=EDGE_CURVE('',#5575,#5574,#2958,.T.);
#6807=EDGE_CURVE('',#5576,#5575,#801,.T.);
#6808=EDGE_CURVE('',#5577,#5576,#2959,.T.);
#6809=EDGE_CURVE('',#5578,#5577,#802,.T.);
#6810=EDGE_CURVE('',#5579,#5578,#2960,.T.);
#6811=EDGE_CURVE('',#5573,#5579,#803,.T.);
#6812=EDGE_CURVE('',#5573,#5534,#2961,.T.);
#6813=EDGE_CURVE('',#5536,#5572,#2962,.T.);
#6814=EDGE_CURVE('',#5579,#5535,#2963,.T.);
#6815=EDGE_CURVE('',#5578,#5580,#2964,.T.);
#6816=EDGE_CURVE('',#5580,#5535,#2965,.T.);
#6817=EDGE_CURVE('',#5577,#5581,#2966,.T.);
#6818=EDGE_CURVE('',#5581,#5580,#804,.T.);
#6819=EDGE_CURVE('',#5576,#5582,#2967,.T.);
#6820=EDGE_CURVE('',#5582,#5581,#2968,.T.);
#6821=EDGE_CURVE('',#5575,#5539,#2969,.T.);
#6822=EDGE_CURVE('',#5539,#5582,#805,.T.);
#6823=EDGE_CURVE('',#5574,#5538,#2970,.T.);
#6824=EDGE_CURVE('',#5582,#5532,#2971,.T.);
#6825=EDGE_CURVE('',#5583,#5583,#806,.T.);
#6826=EDGE_CURVE('',#5583,#5537,#2972,.T.);
#6827=EDGE_CURVE('',#5581,#5530,#2973,.T.);
#6828=EDGE_CURVE('',#5580,#5528,#2974,.T.);
#6829=EDGE_CURVE('',#5567,#5554,#2975,.T.);
#6830=EDGE_CURVE('',#5565,#5553,#2976,.T.);
#6831=EDGE_CURVE('',#5584,#5585,#88,.T.);
#6832=EDGE_CURVE('',#5586,#5585,#89,.T.);
#6833=EDGE_CURVE('',#5586,#5587,#90,.T.);
#6834=EDGE_CURVE('',#5587,#5584,#2977,.T.);
#6835=EDGE_CURVE('',#5588,#5589,#91,.T.);
#6836=EDGE_CURVE('',#5590,#5589,#92,.T.);
#6837=EDGE_CURVE('',#5590,#5591,#93,.T.);
#6838=EDGE_CURVE('',#5591,#5588,#2978,.T.);
#6839=EDGE_CURVE('',#5589,#5592,#94,.T.);
#6840=EDGE_CURVE('',#5592,#5593,#2979,.T.);
#6841=EDGE_CURVE('',#5593,#5590,#95,.T.);
#6842=EDGE_CURVE('',#5594,#5595,#2980,.T.);
#6843=EDGE_CURVE('',#5595,#5596,#807,.T.);
#6844=EDGE_CURVE('',#5596,#5597,#2981,.T.);
#6845=EDGE_CURVE('',#5597,#5594,#808,.T.);
#6846=EDGE_CURVE('',#5594,#5593,#96,.T.);
#6847=EDGE_CURVE('',#5592,#5595,#97,.T.);
#6848=EDGE_CURVE('',#5585,#5598,#98,.T.);
#6849=EDGE_CURVE('',#5598,#5599,#2982,.T.);
#6850=EDGE_CURVE('',#5599,#5586,#99,.T.);
#6851=EDGE_CURVE('',#5598,#5597,#100,.T.);
#6852=EDGE_CURVE('',#5596,#5599,#101,.T.);
#6853=EDGE_CURVE('',#5584,#5600,#2983,.T.);
#6854=EDGE_CURVE('',#5601,#5600,#102,.T.);
#6855=EDGE_CURVE('',#5602,#5601,#103,.T.);
#6856=EDGE_CURVE('',#5602,#5598,#2984,.T.);
#6857=EDGE_CURVE('',#5587,#5603,#2985,.T.);
#6858=EDGE_CURVE('',#5604,#5603,#2986,.T.);
#6859=EDGE_CURVE('',#5605,#5604,#2987,.T.);
#6860=EDGE_CURVE('',#5606,#5605,#2988,.T.);
#6861=EDGE_CURVE('',#5607,#5606,#2989,.T.);
#6862=EDGE_CURVE('',#5600,#5607,#2990,.T.);
#6863=EDGE_CURVE('',#5588,#5608,#2991,.T.);
#6864=EDGE_CURVE('',#5609,#5608,#104,.T.);
#6865=EDGE_CURVE('',#5610,#5609,#105,.T.);
#6866=EDGE_CURVE('',#5611,#5610,#106,.T.);
#6867=EDGE_CURVE('',#5612,#5611,#809,.T.);
#6868=EDGE_CURVE('',#5613,#5612,#107,.T.);
#6869=EDGE_CURVE('',#5614,#5613,#108,.T.);
#6870=EDGE_CURVE('',#5603,#5614,#109,.T.);
#6871=EDGE_CURVE('',#5615,#5616,#110,.T.);
#6872=EDGE_CURVE('',#5617,#5616,#111,.T.);
#6873=EDGE_CURVE('',#5617,#5618,#112,.T.);
#6874=EDGE_CURVE('',#5618,#5615,#2992,.T.);
#6875=EDGE_CURVE('',#5607,#5619,#113,.T.);
#6876=EDGE_CURVE('',#5601,#5619,#114,.T.);
#6877=EDGE_CURVE('',#5619,#5620,#115,.T.);
#6878=EDGE_CURVE('',#5620,#5602,#2993,.T.);
#6879=EDGE_CURVE('',#5621,#5622,#2994,.T.);
#6880=EDGE_CURVE('',#5622,#5623,#810,.T.);
#6881=EDGE_CURVE('',#5623,#5624,#2995,.T.);
#6882=EDGE_CURVE('',#5624,#5621,#811,.T.);
#6883=EDGE_CURVE('',#5621,#5602,#116,.T.);
#6884=EDGE_CURVE('',#5620,#5622,#117,.T.);
#6885=EDGE_CURVE('',#5616,#5625,#118,.T.);
#6886=EDGE_CURVE('',#5625,#5626,#2996,.T.);
#6887=EDGE_CURVE('',#5626,#5617,#119,.T.);
#6888=EDGE_CURVE('',#5625,#5624,#120,.T.);
#6889=EDGE_CURVE('',#5623,#5626,#121,.T.);
#6890=EDGE_CURVE('',#5627,#5625,#2997,.T.);
#6891=EDGE_CURVE('',#5628,#5627,#812,.T.);
#6892=EDGE_CURVE('',#5629,#5628,#2998,.T.);
#6893=EDGE_CURVE('',#5630,#5629,#813,.T.);
#6894=EDGE_CURVE('',#5593,#5630,#2999,.T.);
#6895=EDGE_CURVE('',#5605,#5631,#122,.T.);
#6896=EDGE_CURVE('',#5632,#5631,#123,.T.);
#6897=EDGE_CURVE('',#5632,#5606,#124,.T.);
#6898=EDGE_CURVE('',#5633,#5634,#125,.T.);
#6899=EDGE_CURVE('',#5635,#5634,#126,.T.);
#6900=EDGE_CURVE('',#5635,#5636,#127,.T.);
#6901=EDGE_CURVE('',#5636,#5633,#3000,.T.);
#6902=EDGE_CURVE('',#5634,#5637,#128,.T.);
#6903=EDGE_CURVE('',#5637,#5638,#3001,.T.);
#6904=EDGE_CURVE('',#5638,#5635,#129,.T.);
#6905=EDGE_CURVE('',#5639,#5640,#3002,.T.);
#6906=EDGE_CURVE('',#5640,#5641,#814,.T.);
#6907=EDGE_CURVE('',#5641,#5642,#3003,.T.);
#6908=EDGE_CURVE('',#5642,#5639,#815,.T.);
#6909=EDGE_CURVE('',#5641,#5638,#130,.T.);
#6910=EDGE_CURVE('',#5637,#5642,#131,.T.);
#6911=EDGE_CURVE('',#5631,#5643,#132,.T.);
#6912=EDGE_CURVE('',#5643,#5644,#3004,.T.);
#6913=EDGE_CURVE('',#5644,#5632,#133,.T.);
#6914=EDGE_CURVE('',#5643,#5640,#134,.T.);
#6915=EDGE_CURVE('',#5639,#5644,#135,.T.);
#6916=EDGE_CURVE('',#5645,#5604,#136,.T.);
#6917=EDGE_CURVE('',#5646,#5645,#137,.T.);
#6918=EDGE_CURVE('',#5646,#5643,#3005,.T.);
#6919=EDGE_CURVE('',#5618,#5633,#3006,.T.);
#6920=EDGE_CURVE('',#5647,#5648,#138,.T.);
#6921=EDGE_CURVE('',#5609,#5648,#139,.T.);
#6922=EDGE_CURVE('',#5608,#5647,#3007,.T.);
#6923=EDGE_CURVE('',#5645,#5614,#140,.T.);
#6924=EDGE_CURVE('',#5613,#5646,#3008,.T.);
#6925=EDGE_CURVE('',#5611,#5649,#3009,.T.);
#6926=EDGE_CURVE('',#5649,#5650,#816,.T.);
#6927=EDGE_CURVE('',#5650,#5612,#3010,.T.);
#6928=EDGE_CURVE('',#5650,#5646,#141,.T.);
#6929=EDGE_CURVE('',#5648,#5651,#142,.T.);
#6930=EDGE_CURVE('',#5651,#5610,#3011,.T.);
#6931=EDGE_CURVE('',#5651,#5649,#143,.T.);
#6932=EDGE_CURVE('',#5652,#5651,#3012,.T.);
#6933=EDGE_CURVE('',#5652,#5653,#817,.T.);
#6934=EDGE_CURVE('',#5654,#5653,#3013,.T.);
#6935=EDGE_CURVE('',#5654,#5655,#818,.T.);
#6936=EDGE_CURVE('',#5638,#5655,#3014,.T.);
#6937=EDGE_CURVE('',#5647,#5656,#3015,.T.);
#6938=EDGE_CURVE('',#5656,#5652,#144,.T.);
#6939=EDGE_CURVE('',#5657,#5656,#3016,.T.);
#6940=EDGE_CURVE('',#5630,#5657,#145,.T.);
#6941=EDGE_CURVE('',#5658,#5629,#146,.T.);
#6942=EDGE_CURVE('',#5658,#5659,#3017,.T.);
#6943=EDGE_CURVE('',#5653,#5659,#147,.T.);
#6944=EDGE_CURVE('',#5657,#5591,#3018,.T.);
#6945=EDGE_CURVE('',#5660,#5654,#148,.T.);
#6946=EDGE_CURVE('',#5659,#5660,#3019,.T.);
#6947=EDGE_CURVE('',#5661,#5660,#3020,.T.);
#6948=EDGE_CURVE('',#5628,#5661,#149,.T.);
#6949=EDGE_CURVE('',#5662,#5627,#150,.T.);
#6950=EDGE_CURVE('',#5662,#5663,#3021,.T.);
#6951=EDGE_CURVE('',#5655,#5663,#151,.T.);
#6952=EDGE_CURVE('',#5661,#5658,#3022,.T.);
#6953=EDGE_CURVE('',#5663,#5636,#3023,.T.);
#6954=EDGE_CURVE('',#5615,#5662,#3024,.T.);
#6955=EDGE_CURVE('',#5664,#5665,#152,.T.);
#6956=EDGE_CURVE('',#5666,#5665,#153,.T.);
#6957=EDGE_CURVE('',#5666,#5667,#154,.T.);
#6958=EDGE_CURVE('',#5667,#5664,#3025,.T.);
#6959=EDGE_CURVE('',#5668,#5669,#155,.T.);
#6960=EDGE_CURVE('',#5670,#5669,#156,.T.);
#6961=EDGE_CURVE('',#5670,#5671,#157,.T.);
#6962=EDGE_CURVE('',#5671,#5668,#3026,.T.);
#6963=EDGE_CURVE('',#5669,#5672,#158,.T.);
#6964=EDGE_CURVE('',#5672,#5673,#3027,.T.);
#6965=EDGE_CURVE('',#5673,#5670,#159,.T.);
#6966=EDGE_CURVE('',#5674,#5675,#3028,.T.);
#6967=EDGE_CURVE('',#5675,#5673,#3029,.T.);
#6968=EDGE_CURVE('',#5672,#5674,#3030,.T.);
#6969=EDGE_CURVE('',#5665,#5675,#160,.T.);
#6970=EDGE_CURVE('',#5674,#5666,#161,.T.);
#6971=EDGE_CURVE('',#5674,#5676,#3031,.T.);
#6972=EDGE_CURVE('',#5677,#5676,#162,.T.);
#6973=EDGE_CURVE('',#5678,#5677,#163,.T.);
#6974=EDGE_CURVE('',#5678,#5667,#3032,.T.);
#6975=EDGE_CURVE('',#5679,#5672,#3033,.T.);
#6976=EDGE_CURVE('',#5676,#5679,#3034,.T.);
#6977=EDGE_CURVE('',#5668,#5680,#3035,.T.);
#6978=EDGE_CURVE('',#5681,#5680,#164,.T.);
#6979=EDGE_CURVE('',#5679,#5681,#165,.T.);
#6980=EDGE_CURVE('',#5682,#5671,#3036,.T.);
#6981=EDGE_CURVE('',#5683,#5682,#3037,.T.);
#6982=EDGE_CURVE('',#5684,#5683,#3038,.T.);
#6983=EDGE_CURVE('',#5685,#5684,#3039,.T.);
#6984=EDGE_CURVE('',#5686,#5685,#3040,.T.);
#6985=EDGE_CURVE('',#5680,#5686,#3041,.T.);
#6986=EDGE_CURVE('',#5687,#5677,#166,.T.);
#6987=EDGE_CURVE('',#5687,#5688,#167,.T.);
#6988=EDGE_CURVE('',#5688,#5678,#3042,.T.);
#6989=EDGE_CURVE('',#5686,#5689,#168,.T.);
#6990=EDGE_CURVE('',#5681,#5689,#169,.T.);
#6991=EDGE_CURVE('',#5689,#5690,#170,.T.);
#6992=EDGE_CURVE('',#5690,#5679,#3043,.T.);
#6993=EDGE_CURVE('',#5691,#5676,#3044,.T.);
#6994=EDGE_CURVE('',#5690,#5691,#3045,.T.);
#6995=EDGE_CURVE('',#5691,#5687,#171,.T.);
#6996=EDGE_CURVE('',#5691,#5692,#3046,.T.);
#6997=EDGE_CURVE('',#5693,#5692,#172,.T.);
#6998=EDGE_CURVE('',#5694,#5693,#173,.T.);
#6999=EDGE_CURVE('',#5694,#5688,#3047,.T.);
#7000=EDGE_CURVE('',#5695,#5690,#3048,.T.);
#7001=EDGE_CURVE('',#5692,#5695,#3049,.T.);
#7002=EDGE_CURVE('',#5696,#5685,#174,.T.);
#7003=EDGE_CURVE('',#5695,#5696,#175,.T.);
#7004=EDGE_CURVE('',#5684,#5697,#176,.T.);
#7005=EDGE_CURVE('',#5696,#5697,#177,.T.);
#7006=EDGE_CURVE('',#5698,#5693,#178,.T.);
#7007=EDGE_CURVE('',#5698,#5699,#179,.T.);
#7008=EDGE_CURVE('',#5699,#5694,#3050,.T.);
#7009=EDGE_CURVE('',#5692,#5700,#3051,.T.);
#7010=EDGE_CURVE('',#5700,#5698,#180,.T.);
#7011=EDGE_CURVE('',#5695,#5701,#3052,.T.);
#7012=EDGE_CURVE('',#5701,#5700,#3053,.T.);
#7013=EDGE_CURVE('',#5697,#5701,#181,.T.);
#7014=EDGE_CURVE('',#5682,#5702,#182,.T.);
#7015=EDGE_CURVE('',#5703,#5702,#183,.T.);
#7016=EDGE_CURVE('',#5703,#5683,#184,.T.);
#7017=EDGE_CURVE('',#5704,#5705,#185,.T.);
#7018=EDGE_CURVE('',#5706,#5705,#186,.T.);
#7019=EDGE_CURVE('',#5706,#5707,#187,.T.);
#7020=EDGE_CURVE('',#5707,#5704,#3054,.T.);
#7021=EDGE_CURVE('',#5705,#5708,#188,.T.);
#7022=EDGE_CURVE('',#5708,#5709,#3055,.T.);
#7023=EDGE_CURVE('',#5709,#5706,#189,.T.);
#7024=EDGE_CURVE('',#5708,#5710,#3056,.T.);
#7025=EDGE_CURVE('',#5710,#5711,#3057,.T.);
#7026=EDGE_CURVE('',#5711,#5709,#3058,.T.);
#7027=EDGE_CURVE('',#5702,#5711,#190,.T.);
#7028=EDGE_CURVE('',#5710,#5703,#191,.T.);
#7029=EDGE_CURVE('',#5710,#5701,#3059,.T.);
#7030=EDGE_CURVE('',#5700,#5708,#3060,.T.);
#7031=EDGE_CURVE('',#5704,#5699,#3061,.T.);
#7032=EDGE_CURVE('',#5664,#5707,#3062,.T.);
#7033=EDGE_CURVE('',#5709,#5675,#3063,.T.);
#7034=EDGE_CURVE('',#5673,#5711,#3064,.T.);
#7035=EDGE_CURVE('',#5712,#5712,#819,.T.);
#7036=EDGE_CURVE('',#5712,#5713,#3065,.T.);
#7037=EDGE_CURVE('',#5713,#5713,#820,.T.);
#7038=EDGE_CURVE('',#5713,#5714,#3066,.T.);
#7039=EDGE_CURVE('',#5714,#5714,#821,.T.);
#7040=EDGE_CURVE('',#5715,#5716,#3067,.T.);
#7041=EDGE_CURVE('',#5715,#5717,#3068,.T.);
#7042=EDGE_CURVE('',#5718,#5717,#3069,.T.);
#7043=EDGE_CURVE('',#5716,#5718,#3070,.T.);
#7044=EDGE_CURVE('',#5719,#5719,#822,.T.);
#7045=EDGE_CURVE('',#5719,#5714,#3071,.T.);
#7046=EDGE_CURVE('',#5720,#5721,#3072,.T.);
#7047=EDGE_CURVE('',#5720,#5722,#3073,.T.);
#7048=EDGE_CURVE('',#5723,#5722,#3074,.T.);
#7049=EDGE_CURVE('',#5721,#5723,#3075,.T.);
#7050=EDGE_CURVE('',#5724,#5725,#3076,.T.);
#7051=EDGE_CURVE('',#5725,#5726,#3077,.T.);
#7052=EDGE_CURVE('',#5726,#5727,#3078,.T.);
#7053=EDGE_CURVE('',#5727,#5724,#3079,.T.);
#7054=EDGE_CURVE('',#5728,#5729,#3080,.T.);
#7055=EDGE_CURVE('',#5729,#5725,#823,.T.);
#7056=EDGE_CURVE('',#5724,#5728,#824,.T.);
#7057=EDGE_CURVE('',#5730,#5731,#3081,.T.);
#7058=EDGE_CURVE('',#5731,#5729,#3082,.T.);
#7059=EDGE_CURVE('',#5728,#5730,#3083,.T.);
#7060=EDGE_CURVE('',#5720,#5732,#3084,.T.);
#7061=EDGE_CURVE('',#5732,#5731,#825,.T.);
#7062=EDGE_CURVE('',#5730,#5720,#826,.T.);
#7063=EDGE_CURVE('',#5721,#5733,#3085,.T.);
#7064=EDGE_CURVE('',#5733,#5732,#3086,.T.);
#7065=EDGE_CURVE('',#5734,#5735,#3087,.T.);
#7066=EDGE_CURVE('',#5735,#5733,#827,.T.);
#7067=EDGE_CURVE('',#5721,#5734,#828,.T.);
#7068=EDGE_CURVE('',#5736,#5737,#3088,.T.);
#7069=EDGE_CURVE('',#5737,#5735,#3089,.T.);
#7070=EDGE_CURVE('',#5734,#5736,#3090,.T.);
#7071=EDGE_CURVE('',#5726,#5737,#829,.T.);
#7072=EDGE_CURVE('',#5736,#5727,#830,.T.);
#7073=EDGE_CURVE('',#5730,#5738,#3091,.T.);
#7074=EDGE_CURVE('',#5722,#5738,#831,.T.);
#7075=EDGE_CURVE('',#5728,#5739,#3092,.T.);
#7076=EDGE_CURVE('',#5738,#5739,#3093,.T.);
#7077=EDGE_CURVE('',#5724,#5740,#3094,.T.);
#7078=EDGE_CURVE('',#5739,#5740,#832,.T.);
#7079=EDGE_CURVE('',#5727,#5741,#3095,.T.);
#7080=EDGE_CURVE('',#5740,#5741,#3096,.T.);
#7081=EDGE_CURVE('',#5742,#5743,#833,.T.);
#7082=EDGE_CURVE('',#5744,#5742,#3097,.T.);
#7083=EDGE_CURVE('',#5745,#5744,#834,.T.);
#7084=EDGE_CURVE('',#5746,#5745,#3098,.T.);
#7085=EDGE_CURVE('',#5747,#5746,#835,.T.);
#7086=EDGE_CURVE('',#5748,#5747,#3099,.T.);
#7087=EDGE_CURVE('',#5749,#5748,#836,.T.);
#7088=EDGE_CURVE('',#5743,#5749,#3100,.T.);
#7089=EDGE_CURVE('',#5750,#5742,#3101,.T.);
#7090=EDGE_CURVE('',#5743,#5716,#3102,.T.);
#7091=EDGE_CURVE('',#5716,#5750,#837,.T.);
#7092=EDGE_CURVE('',#5750,#5751,#3103,.T.);
#7093=EDGE_CURVE('',#5751,#5744,#3104,.T.);
#7094=EDGE_CURVE('',#5752,#5745,#3105,.T.);
#7095=EDGE_CURVE('',#5751,#5752,#838,.T.);
#7096=EDGE_CURVE('',#5752,#5753,#3106,.T.);
#7097=EDGE_CURVE('',#5753,#5746,#3107,.T.);
#7098=EDGE_CURVE('',#5754,#5747,#3108,.T.);
#7099=EDGE_CURVE('',#5753,#5754,#839,.T.);
#7100=EDGE_CURVE('',#5754,#5755,#3109,.T.);
#7101=EDGE_CURVE('',#5755,#5748,#3110,.T.);
#7102=EDGE_CURVE('',#5715,#5749,#3111,.T.);
#7103=EDGE_CURVE('',#5755,#5715,#840,.T.);
#7104=EDGE_CURVE('',#5752,#5756,#3112,.T.);
#7105=EDGE_CURVE('',#5757,#5756,#3113,.T.);
#7106=EDGE_CURVE('',#5753,#5757,#3114,.T.);
#7107=EDGE_CURVE('',#5751,#5758,#3115,.T.);
#7108=EDGE_CURVE('',#5756,#5758,#841,.T.);
#7109=EDGE_CURVE('',#5750,#5759,#3116,.T.);
#7110=EDGE_CURVE('',#5758,#5759,#3117,.T.);
#7111=EDGE_CURVE('',#5759,#5718,#842,.T.);
#7112=EDGE_CURVE('',#5756,#5760,#3118,.T.);
#7113=EDGE_CURVE('',#5760,#5761,#3119,.T.);
#7114=EDGE_CURVE('',#5761,#5757,#3120,.T.);
#7115=EDGE_CURVE('',#5758,#5762,#3121,.T.);
#7116=EDGE_CURVE('',#5762,#5760,#843,.T.);
#7117=EDGE_CURVE('',#5759,#5763,#3122,.T.);
#7118=EDGE_CURVE('',#5763,#5762,#3123,.T.);
#7119=EDGE_CURVE('',#5718,#5764,#3124,.T.);
#7120=EDGE_CURVE('',#5764,#5763,#844,.T.);
#7121=EDGE_CURVE('',#5717,#5765,#3125,.T.);
#7122=EDGE_CURVE('',#5765,#5764,#3126,.T.);
#7123=EDGE_CURVE('',#5766,#5767,#3127,.T.);
#7124=EDGE_CURVE('',#5767,#5765,#845,.T.);
#7125=EDGE_CURVE('',#5717,#5766,#846,.T.);
#7126=EDGE_CURVE('',#5768,#5769,#3128,.T.);
#7127=EDGE_CURVE('',#5769,#5767,#3129,.T.);
#7128=EDGE_CURVE('',#5766,#5768,#3130,.T.);
#7129=EDGE_CURVE('',#5761,#5769,#847,.T.);
#7130=EDGE_CURVE('',#5768,#5757,#848,.T.);
#7131=EDGE_CURVE('',#5770,#5771,#3131,.T.);
#7132=EDGE_CURVE('',#5772,#5770,#849,.T.);
#7133=EDGE_CURVE('',#5773,#5772,#3132,.T.);
#7134=EDGE_CURVE('',#5774,#5773,#850,.T.);
#7135=EDGE_CURVE('',#5775,#5774,#3133,.T.);
#7136=EDGE_CURVE('',#5776,#5775,#851,.T.);
#7137=EDGE_CURVE('',#5777,#5776,#3134,.T.);
#7138=EDGE_CURVE('',#5771,#5777,#852,.T.);
#7139=EDGE_CURVE('',#5739,#5770,#3135,.T.);
#7140=EDGE_CURVE('',#5771,#5738,#3136,.T.);
#7141=EDGE_CURVE('',#5740,#5772,#3137,.T.);
#7142=EDGE_CURVE('',#5741,#5773,#3138,.T.);
#7143=EDGE_CURVE('',#5778,#5774,#3139,.T.);
#7144=EDGE_CURVE('',#5741,#5778,#853,.T.);
#7145=EDGE_CURVE('',#5779,#5775,#3140,.T.);
#7146=EDGE_CURVE('',#5778,#5779,#3141,.T.);
#7147=EDGE_CURVE('',#5723,#5776,#3142,.T.);
#7148=EDGE_CURVE('',#5779,#5723,#854,.T.);
#7149=EDGE_CURVE('',#5722,#5777,#3143,.T.);
#7150=EDGE_CURVE('',#5736,#5778,#3144,.T.);
#7151=EDGE_CURVE('',#5734,#5779,#3145,.T.);
#7152=EDGE_CURVE('',#5754,#5768,#3146,.T.);
#7153=EDGE_CURVE('',#5755,#5766,#3147,.T.);
#7154=EDGE_CURVE('',#5780,#5780,#855,.T.);
#7155=EDGE_CURVE('',#5780,#5781,#3148,.T.);
#7156=EDGE_CURVE('',#5781,#5781,#856,.T.);
#7157=EDGE_CURVE('',#5782,#5783,#3149,.T.);
#7158=EDGE_CURVE('',#5782,#5784,#3150,.T.);
#7159=EDGE_CURVE('',#5785,#5784,#3151,.T.);
#7160=EDGE_CURVE('',#5783,#5785,#3152,.T.);
#7161=EDGE_CURVE('',#5786,#5786,#857,.T.);
#7162=EDGE_CURVE('',#5787,#5787,#858,.T.);
#7163=EDGE_CURVE('',#5788,#5788,#859,.T.);
#7164=EDGE_CURVE('',#5789,#5789,#860,.T.);
#7165=EDGE_CURVE('',#5790,#5790,#861,.T.);
#7166=EDGE_CURVE('',#5791,#5791,#862,.T.);
#7167=EDGE_CURVE('',#5791,#5781,#3153,.T.);
#7168=EDGE_CURVE('',#5786,#5792,#3154,.T.);
#7169=EDGE_CURVE('',#5792,#5792,#863,.T.);
#7170=EDGE_CURVE('',#5793,#5793,#864,.T.);
#7171=EDGE_CURVE('',#5793,#5792,#3155,.T.);
#7172=EDGE_CURVE('',#5790,#5794,#3156,.T.);
#7173=EDGE_CURVE('',#5794,#5794,#865,.T.);
#7174=EDGE_CURVE('',#5795,#5795,#866,.T.);
#7175=EDGE_CURVE('',#5795,#5794,#3157,.T.);
#7176=EDGE_CURVE('',#5787,#5796,#3158,.T.);
#7177=EDGE_CURVE('',#5796,#5796,#867,.T.);
#7178=EDGE_CURVE('',#5797,#5797,#868,.T.);
#7179=EDGE_CURVE('',#5797,#5796,#3159,.T.);
#7180=EDGE_CURVE('',#5789,#5798,#3160,.T.);
#7181=EDGE_CURVE('',#5798,#5798,#869,.T.);
#7182=EDGE_CURVE('',#5799,#5799,#870,.T.);
#7183=EDGE_CURVE('',#5799,#5798,#3161,.T.);
#7184=EDGE_CURVE('',#5788,#5800,#3162,.T.);
#7185=EDGE_CURVE('',#5800,#5800,#871,.T.);
#7186=EDGE_CURVE('',#5801,#5801,#872,.T.);
#7187=EDGE_CURVE('',#5801,#5800,#3163,.T.);
#7188=EDGE_CURVE('',#5802,#5802,#873,.T.);
#7189=EDGE_CURVE('',#5802,#5803,#3164,.T.);
#7190=EDGE_CURVE('',#5803,#5803,#874,.T.);
#7191=EDGE_CURVE('',#5804,#5805,#3165,.T.);
#7192=EDGE_CURVE('',#5804,#5806,#3166,.T.);
#7193=EDGE_CURVE('',#5807,#5806,#3167,.T.);
#7194=EDGE_CURVE('',#5805,#5807,#3168,.T.);
#7195=EDGE_CURVE('',#5808,#5808,#875,.T.);
#7196=EDGE_CURVE('',#5809,#5809,#876,.T.);
#7197=EDGE_CURVE('',#5810,#5810,#877,.T.);
#7198=EDGE_CURVE('',#5811,#5811,#878,.T.);
#7199=EDGE_CURVE('',#5812,#5812,#879,.T.);
#7200=EDGE_CURVE('',#5813,#5813,#880,.T.);
#7201=EDGE_CURVE('',#5814,#5814,#881,.T.);
#7202=EDGE_CURVE('',#5814,#5803,#3169,.T.);
#7203=EDGE_CURVE('',#5815,#5804,#3170,.T.);
#7204=EDGE_CURVE('',#5805,#5816,#3171,.T.);
#7205=EDGE_CURVE('',#5816,#5815,#3172,.T.);
#7206=EDGE_CURVE('',#5817,#5818,#3173,.T.);
#7207=EDGE_CURVE('',#5818,#5804,#882,.T.);
#7208=EDGE_CURVE('',#5815,#5817,#883,.T.);
#7209=EDGE_CURVE('',#5819,#5820,#3174,.T.);
#7210=EDGE_CURVE('',#5820,#5818,#3175,.T.);
#7211=EDGE_CURVE('',#5817,#5819,#3176,.T.);
#7212=EDGE_CURVE('',#5821,#5822,#3177,.T.);
#7213=EDGE_CURVE('',#5822,#5820,#884,.T.);
#7214=EDGE_CURVE('',#5819,#5821,#885,.T.);
#7215=EDGE_CURVE('',#5823,#5824,#3178,.T.);
#7216=EDGE_CURVE('',#5824,#5822,#3179,.T.);
#7217=EDGE_CURVE('',#5821,#5823,#3180,.T.);
#7218=EDGE_CURVE('',#5825,#5783,#3181,.T.);
#7219=EDGE_CURVE('',#5783,#5824,#886,.T.);
#7220=EDGE_CURVE('',#5823,#5825,#887,.T.);
#7221=EDGE_CURVE('',#5826,#5782,#3182,.T.);
#7222=EDGE_CURVE('',#5825,#5826,#3183,.T.);
#7223=EDGE_CURVE('',#5805,#5782,#888,.T.);
#7224=EDGE_CURVE('',#5826,#5816,#889,.T.);
#7225=EDGE_CURVE('',#5827,#5785,#890,.T.);
#7226=EDGE_CURVE('',#5824,#5827,#3184,.T.);
#7227=EDGE_CURVE('',#5784,#5807,#891,.T.);
#7228=EDGE_CURVE('',#5828,#5829,#3185,.T.);
#7229=EDGE_CURVE('',#5830,#5828,#892,.T.);
#7230=EDGE_CURVE('',#5831,#5830,#3186,.T.);
#7231=EDGE_CURVE('',#5832,#5831,#893,.T.);
#7232=EDGE_CURVE('',#5833,#5832,#3187,.T.);
#7233=EDGE_CURVE('',#5834,#5833,#894,.T.);
#7234=EDGE_CURVE('',#5835,#5834,#3188,.T.);
#7235=EDGE_CURVE('',#5829,#5835,#895,.T.);
#7236=EDGE_CURVE('',#5813,#5836,#3189,.T.);
#7237=EDGE_CURVE('',#5836,#5836,#896,.T.);
#7238=EDGE_CURVE('',#5837,#5837,#897,.T.);
#7239=EDGE_CURVE('',#5837,#5836,#3190,.T.);
#7240=EDGE_CURVE('',#5808,#5838,#3191,.T.);
#7241=EDGE_CURVE('',#5838,#5838,#898,.T.);
#7242=EDGE_CURVE('',#5839,#5839,#899,.T.);
#7243=EDGE_CURVE('',#5839,#5838,#3192,.T.);
#7244=EDGE_CURVE('',#5812,#5840,#3193,.T.);
#7245=EDGE_CURVE('',#5840,#5840,#900,.T.);
#7246=EDGE_CURVE('',#5841,#5841,#901,.T.);
#7247=EDGE_CURVE('',#5841,#5840,#3194,.T.);
#7248=EDGE_CURVE('',#5809,#5842,#3195,.T.);
#7249=EDGE_CURVE('',#5842,#5842,#902,.T.);
#7250=EDGE_CURVE('',#5843,#5843,#903,.T.);
#7251=EDGE_CURVE('',#5843,#5842,#3196,.T.);
#7252=EDGE_CURVE('',#5811,#5844,#3197,.T.);
#7253=EDGE_CURVE('',#5844,#5844,#904,.T.);
#7254=EDGE_CURVE('',#5845,#5845,#905,.T.);
#7255=EDGE_CURVE('',#5845,#5844,#3198,.T.);
#7256=EDGE_CURVE('',#5810,#5846,#3199,.T.);
#7257=EDGE_CURVE('',#5846,#5846,#906,.T.);
#7258=EDGE_CURVE('',#5847,#5847,#907,.T.);
#7259=EDGE_CURVE('',#5847,#5846,#3200,.T.);
#7260=EDGE_CURVE('',#5848,#5848,#908,.T.);
#7261=EDGE_CURVE('',#5848,#5837,#3201,.T.);
#7262=EDGE_CURVE('',#5849,#5850,#3202,.T.);
#7263=EDGE_CURVE('',#5849,#5851,#3203,.T.);
#7264=EDGE_CURVE('',#5852,#5851,#3204,.T.);
#7265=EDGE_CURVE('',#5850,#5852,#3205,.T.);
#7266=EDGE_CURVE('',#5853,#5853,#909,.T.);
#7267=EDGE_CURVE('',#5854,#5854,#910,.T.);
#7268=EDGE_CURVE('',#5855,#5855,#911,.T.);
#7269=EDGE_CURVE('',#5856,#5856,#912,.T.);
#7270=EDGE_CURVE('',#5857,#5857,#913,.T.);
#7271=EDGE_CURVE('',#5858,#5858,#914,.T.);
#7272=EDGE_CURVE('',#5853,#5814,#3206,.T.);
#7273=EDGE_CURVE('',#5858,#5839,#3207,.T.);
#7274=EDGE_CURVE('',#5854,#5841,#3208,.T.);
#7275=EDGE_CURVE('',#5857,#5843,#3209,.T.);
#7276=EDGE_CURVE('',#5855,#5845,#3210,.T.);
#7277=EDGE_CURVE('',#5856,#5847,#3211,.T.);
#7278=EDGE_CURVE('',#5829,#5859,#3212,.T.);
#7279=EDGE_CURVE('',#5859,#5860,#3213,.T.);
#7280=EDGE_CURVE('',#5860,#5828,#3214,.T.);
#7281=EDGE_CURVE('',#5835,#5861,#3215,.T.);
#7282=EDGE_CURVE('',#5861,#5859,#915,.T.);
#7283=EDGE_CURVE('',#5834,#5862,#3216,.T.);
#7284=EDGE_CURVE('',#5862,#5861,#3217,.T.);
#7285=EDGE_CURVE('',#5833,#5863,#3218,.T.);
#7286=EDGE_CURVE('',#5863,#5862,#916,.T.);
#7287=EDGE_CURVE('',#5832,#5864,#3219,.T.);
#7288=EDGE_CURVE('',#5864,#5863,#3220,.T.);
#7289=EDGE_CURVE('',#5831,#5850,#3221,.T.);
#7290=EDGE_CURVE('',#5850,#5864,#917,.T.);
#7291=EDGE_CURVE('',#5830,#5849,#3222,.T.);
#7292=EDGE_CURVE('',#5860,#5849,#918,.T.);
#7293=EDGE_CURVE('',#5865,#5852,#919,.T.);
#7294=EDGE_CURVE('',#5864,#5865,#3223,.T.);
#7295=EDGE_CURVE('',#5860,#5866,#3224,.T.);
#7296=EDGE_CURVE('',#5851,#5866,#920,.T.);
#7297=EDGE_CURVE('',#5859,#5867,#3225,.T.);
#7298=EDGE_CURVE('',#5866,#5867,#3226,.T.);
#7299=EDGE_CURVE('',#5868,#5868,#921,.T.);
#7300=EDGE_CURVE('',#5869,#5869,#922,.T.);
#7301=EDGE_CURVE('',#5870,#5870,#923,.T.);
#7302=EDGE_CURVE('',#5871,#5871,#924,.T.);
#7303=EDGE_CURVE('',#5872,#5872,#925,.T.);
#7304=EDGE_CURVE('',#5873,#5873,#926,.T.);
#7305=EDGE_CURVE('',#5868,#5801,#3227,.T.);
#7306=EDGE_CURVE('',#5873,#5799,#3228,.T.);
#7307=EDGE_CURVE('',#5869,#5797,#3229,.T.);
#7308=EDGE_CURVE('',#5872,#5795,#3230,.T.);
#7309=EDGE_CURVE('',#5870,#5793,#3231,.T.);
#7310=EDGE_CURVE('',#5871,#5791,#3232,.T.);
#7311=EDGE_CURVE('',#5851,#5874,#3233,.T.);
#7312=EDGE_CURVE('',#5874,#5875,#3234,.T.);
#7313=EDGE_CURVE('',#5875,#5852,#3235,.T.);
#7314=EDGE_CURVE('',#5866,#5876,#3236,.T.);
#7315=EDGE_CURVE('',#5876,#5874,#927,.T.);
#7316=EDGE_CURVE('',#5867,#5877,#3237,.T.);
#7317=EDGE_CURVE('',#5877,#5876,#3238,.T.);
#7318=EDGE_CURVE('',#5878,#5879,#3239,.T.);
#7319=EDGE_CURVE('',#5879,#5877,#928,.T.);
#7320=EDGE_CURVE('',#5867,#5878,#929,.T.);
#7321=EDGE_CURVE('',#5880,#5881,#3240,.T.);
#7322=EDGE_CURVE('',#5881,#5879,#3241,.T.);
#7323=EDGE_CURVE('',#5878,#5880,#3242,.T.);
#7324=EDGE_CURVE('',#5882,#5883,#3243,.T.);
#7325=EDGE_CURVE('',#5883,#5881,#930,.T.);
#7326=EDGE_CURVE('',#5880,#5882,#931,.T.);
#7327=EDGE_CURVE('',#5865,#5884,#3244,.T.);
#7328=EDGE_CURVE('',#5884,#5883,#3245,.T.);
#7329=EDGE_CURVE('',#5882,#5865,#3246,.T.);
#7330=EDGE_CURVE('',#5875,#5884,#932,.T.);
#7331=EDGE_CURVE('',#5861,#5878,#3247,.T.);
#7332=EDGE_CURVE('',#5885,#5886,#3248,.T.);
#7333=EDGE_CURVE('',#5887,#5885,#933,.T.);
#7334=EDGE_CURVE('',#5888,#5887,#3249,.T.);
#7335=EDGE_CURVE('',#5889,#5888,#934,.T.);
#7336=EDGE_CURVE('',#5890,#5889,#3250,.T.);
#7337=EDGE_CURVE('',#5891,#5890,#935,.T.);
#7338=EDGE_CURVE('',#5892,#5891,#3251,.T.);
#7339=EDGE_CURVE('',#5886,#5892,#936,.T.);
#7340=EDGE_CURVE('',#5784,#5885,#3252,.T.);
#7341=EDGE_CURVE('',#5886,#5785,#3253,.T.);
#7342=EDGE_CURVE('',#5807,#5887,#3254,.T.);
#7343=EDGE_CURVE('',#5806,#5888,#3255,.T.);
#7344=EDGE_CURVE('',#5893,#5889,#3256,.T.);
#7345=EDGE_CURVE('',#5806,#5893,#937,.T.);
#7346=EDGE_CURVE('',#5894,#5890,#3257,.T.);
#7347=EDGE_CURVE('',#5893,#5894,#3258,.T.);
#7348=EDGE_CURVE('',#5895,#5891,#3259,.T.);
#7349=EDGE_CURVE('',#5894,#5895,#938,.T.);
#7350=EDGE_CURVE('',#5827,#5892,#3260,.T.);
#7351=EDGE_CURVE('',#5895,#5827,#3261,.T.);
#7352=EDGE_CURVE('',#5818,#5893,#3262,.T.);
#7353=EDGE_CURVE('',#5822,#5895,#3263,.T.);
#7354=EDGE_CURVE('',#5820,#5894,#3264,.T.);
#7355=EDGE_CURVE('',#5863,#5882,#3265,.T.);
#7356=EDGE_CURVE('',#5862,#5880,#3266,.T.);
#7357=EDGE_CURVE('',#5896,#5897,#192,.T.);
#7358=EDGE_CURVE('',#5898,#5897,#193,.T.);
#7359=EDGE_CURVE('',#5898,#5899,#194,.T.);
#7360=EDGE_CURVE('',#5899,#5896,#3267,.T.);
#7361=EDGE_CURVE('',#5900,#5901,#195,.T.);
#7362=EDGE_CURVE('',#5902,#5901,#196,.T.);
#7363=EDGE_CURVE('',#5902,#5903,#197,.T.);
#7364=EDGE_CURVE('',#5903,#5900,#3268,.T.);
#7365=EDGE_CURVE('',#5901,#5904,#198,.T.);
#7366=EDGE_CURVE('',#5904,#5905,#3269,.T.);
#7367=EDGE_CURVE('',#5905,#5902,#199,.T.);
#7368=EDGE_CURVE('',#5906,#5907,#3270,.T.);
#7369=EDGE_CURVE('',#5907,#5908,#939,.T.);
#7370=EDGE_CURVE('',#5908,#5909,#3271,.T.);
#7371=EDGE_CURVE('',#5909,#5906,#940,.T.);
#7372=EDGE_CURVE('',#5908,#5905,#200,.T.);
#7373=EDGE_CURVE('',#5904,#5909,#201,.T.);
#7374=EDGE_CURVE('',#5897,#5910,#202,.T.);
#7375=EDGE_CURVE('',#5910,#5911,#3272,.T.);
#7376=EDGE_CURVE('',#5911,#5898,#203,.T.);
#7377=EDGE_CURVE('',#5910,#5907,#204,.T.);
#7378=EDGE_CURVE('',#5906,#5911,#205,.T.);
#7379=EDGE_CURVE('',#5896,#5912,#3273,.T.);
#7380=EDGE_CURVE('',#5912,#5913,#206,.T.);
#7381=EDGE_CURVE('',#5913,#5910,#3274,.T.);
#7382=EDGE_CURVE('',#5899,#5914,#3275,.T.);
#7383=EDGE_CURVE('',#5915,#5914,#3276,.T.);
#7384=EDGE_CURVE('',#5916,#5915,#3277,.T.);
#7385=EDGE_CURVE('',#5912,#5916,#3278,.T.);
#7386=EDGE_CURVE('',#5900,#5917,#3279,.T.);
#7387=EDGE_CURVE('',#5918,#5917,#207,.T.);
#7388=EDGE_CURVE('',#5919,#5918,#208,.T.);
#7389=EDGE_CURVE('',#5920,#5919,#209,.T.);
#7390=EDGE_CURVE('',#5921,#5920,#941,.T.);
#7391=EDGE_CURVE('',#5922,#5921,#210,.T.);
#7392=EDGE_CURVE('',#5923,#5922,#211,.T.);
#7393=EDGE_CURVE('',#5914,#5923,#212,.T.);
#7394=EDGE_CURVE('',#5924,#5925,#213,.T.);
#7395=EDGE_CURVE('',#5926,#5925,#214,.T.);
#7396=EDGE_CURVE('',#5926,#5927,#215,.T.);
#7397=EDGE_CURVE('',#5927,#5924,#3280,.T.);
#7398=EDGE_CURVE('',#5928,#5929,#216,.T.);
#7399=EDGE_CURVE('',#5930,#5929,#217,.T.);
#7400=EDGE_CURVE('',#5930,#5931,#218,.T.);
#7401=EDGE_CURVE('',#5931,#5928,#3281,.T.);
#7402=EDGE_CURVE('',#5929,#5932,#219,.T.);
#7403=EDGE_CURVE('',#5932,#5933,#3282,.T.);
#7404=EDGE_CURVE('',#5933,#5930,#220,.T.);
#7405=EDGE_CURVE('',#5934,#5935,#3283,.T.);
#7406=EDGE_CURVE('',#5935,#5936,#942,.T.);
#7407=EDGE_CURVE('',#5936,#5937,#3284,.T.);
#7408=EDGE_CURVE('',#5937,#5934,#943,.T.);
#7409=EDGE_CURVE('',#5936,#5933,#221,.T.);
#7410=EDGE_CURVE('',#5932,#5937,#222,.T.);
#7411=EDGE_CURVE('',#5925,#5938,#223,.T.);
#7412=EDGE_CURVE('',#5938,#5939,#3285,.T.);
#7413=EDGE_CURVE('',#5939,#5926,#224,.T.);
#7414=EDGE_CURVE('',#5938,#5935,#225,.T.);
#7415=EDGE_CURVE('',#5934,#5939,#226,.T.);
#7416=EDGE_CURVE('',#5940,#5931,#3286,.T.);
#7417=EDGE_CURVE('',#5940,#5941,#3287,.T.);
#7418=EDGE_CURVE('',#5942,#5941,#3288,.T.);
#7419=EDGE_CURVE('',#5943,#5942,#3289,.T.);
#7420=EDGE_CURVE('',#5928,#5943,#3290,.T.);
#7421=EDGE_CURVE('',#5933,#5944,#3291,.T.);
#7422=EDGE_CURVE('',#5944,#5940,#227,.T.);
#7423=EDGE_CURVE('',#5913,#5945,#944,.T.);
#7424=EDGE_CURVE('',#5946,#5945,#3292,.T.);
#7425=EDGE_CURVE('',#5946,#5944,#945,.T.);
#7426=EDGE_CURVE('',#5905,#5938,#3293,.T.);
#7427=EDGE_CURVE('',#5947,#5948,#228,.T.);
#7428=EDGE_CURVE('',#5918,#5948,#229,.T.);
#7429=EDGE_CURVE('',#5917,#5947,#3294,.T.);
#7430=EDGE_CURVE('',#5949,#5923,#230,.T.);
#7431=EDGE_CURVE('',#5949,#5915,#231,.T.);
#7432=EDGE_CURVE('',#5922,#5950,#3295,.T.);
#7433=EDGE_CURVE('',#5950,#5949,#232,.T.);
#7434=EDGE_CURVE('',#5920,#5951,#3296,.T.);
#7435=EDGE_CURVE('',#5951,#5952,#946,.T.);
#7436=EDGE_CURVE('',#5952,#5921,#3297,.T.);
#7437=EDGE_CURVE('',#5952,#5950,#233,.T.);
#7438=EDGE_CURVE('',#5948,#5953,#234,.T.);
#7439=EDGE_CURVE('',#5953,#5919,#3298,.T.);
#7440=EDGE_CURVE('',#5953,#5951,#235,.T.);
#7441=EDGE_CURVE('',#5947,#5954,#3299,.T.);
#7442=EDGE_CURVE('',#5955,#5954,#236,.T.);
#7443=EDGE_CURVE('',#5956,#5955,#237,.T.);
#7444=EDGE_CURVE('',#5956,#5953,#3300,.T.);
#7445=EDGE_CURVE('',#5924,#5903,#3301,.T.);
#7446=EDGE_CURVE('',#5927,#5957,#3302,.T.);
#7447=EDGE_CURVE('',#5954,#5957,#3303,.T.);
#7448=EDGE_CURVE('',#5942,#5958,#238,.T.);
#7449=EDGE_CURVE('',#5959,#5958,#239,.T.);
#7450=EDGE_CURVE('',#5959,#5943,#240,.T.);
#7451=EDGE_CURVE('',#5957,#5960,#241,.T.);
#7452=EDGE_CURVE('',#5955,#5960,#242,.T.);
#7453=EDGE_CURVE('',#5960,#5961,#243,.T.);
#7454=EDGE_CURVE('',#5961,#5956,#3304,.T.);
#7455=EDGE_CURVE('',#5962,#5963,#3305,.T.);
#7456=EDGE_CURVE('',#5963,#5964,#947,.T.);
#7457=EDGE_CURVE('',#5964,#5965,#3306,.T.);
#7458=EDGE_CURVE('',#5965,#5962,#948,.T.);
#7459=EDGE_CURVE('',#5964,#5956,#244,.T.);
#7460=EDGE_CURVE('',#5961,#5965,#245,.T.);
#7461=EDGE_CURVE('',#5958,#5966,#246,.T.);
#7462=EDGE_CURVE('',#5966,#5967,#3307,.T.);
#7463=EDGE_CURVE('',#5967,#5959,#247,.T.);
#7464=EDGE_CURVE('',#5966,#5963,#248,.T.);
#7465=EDGE_CURVE('',#5962,#5967,#249,.T.);
#7466=EDGE_CURVE('',#5968,#5966,#3308,.T.);
#7467=EDGE_CURVE('',#5968,#5969,#949,.T.);
#7468=EDGE_CURVE('',#5970,#5969,#3309,.T.);
#7469=EDGE_CURVE('',#5970,#5971,#950,.T.);
#7470=EDGE_CURVE('',#5950,#5971,#3310,.T.);
#7471=EDGE_CURVE('',#5941,#5968,#250,.T.);
#7472=EDGE_CURVE('',#5972,#5946,#251,.T.);
#7473=EDGE_CURVE('',#5972,#5973,#3311,.T.);
#7474=EDGE_CURVE('',#5969,#5973,#252,.T.);
#7475=EDGE_CURVE('',#5974,#5970,#253,.T.);
#7476=EDGE_CURVE('',#5973,#5974,#3312,.T.);
#7477=EDGE_CURVE('',#5975,#5974,#3313,.T.);
#7478=EDGE_CURVE('',#5945,#5975,#254,.T.);
#7479=EDGE_CURVE('',#5971,#5916,#255,.T.);
#7480=EDGE_CURVE('',#5975,#5972,#3314,.T.);
#7481=EDGE_CURVE('',#5976,#5977,#256,.T.);
#7482=EDGE_CURVE('',#5978,#5977,#257,.T.);
#7483=EDGE_CURVE('',#5978,#5979,#258,.T.);
#7484=EDGE_CURVE('',#5979,#5976,#3315,.T.);
#7485=EDGE_CURVE('',#5980,#5981,#259,.T.);
#7486=EDGE_CURVE('',#5982,#5981,#260,.T.);
#7487=EDGE_CURVE('',#5982,#5983,#261,.T.);
#7488=EDGE_CURVE('',#5983,#5980,#3316,.T.);
#7489=EDGE_CURVE('',#5981,#5984,#262,.T.);
#7490=EDGE_CURVE('',#5984,#5985,#3317,.T.);
#7491=EDGE_CURVE('',#5985,#5982,#263,.T.);
#7492=EDGE_CURVE('',#5984,#5986,#3318,.T.);
#7493=EDGE_CURVE('',#5986,#5987,#3319,.T.);
#7494=EDGE_CURVE('',#5987,#5985,#3320,.T.);
#7495=EDGE_CURVE('',#5977,#5987,#264,.T.);
#7496=EDGE_CURVE('',#5986,#5978,#265,.T.);
#7497=EDGE_CURVE('',#5988,#5979,#3321,.T.);
#7498=EDGE_CURVE('',#5989,#5988,#3322,.T.);
#7499=EDGE_CURVE('',#5990,#5989,#3323,.T.);
#7500=EDGE_CURVE('',#5991,#5990,#3324,.T.);
#7501=EDGE_CURVE('',#5992,#5991,#3325,.T.);
#7502=EDGE_CURVE('',#5993,#5992,#3326,.T.);
#7503=EDGE_CURVE('',#5976,#5993,#3327,.T.);
#7504=EDGE_CURVE('',#5986,#5994,#3328,.T.);
#7505=EDGE_CURVE('',#5995,#5994,#266,.T.);
#7506=EDGE_CURVE('',#5988,#5995,#267,.T.);
#7507=EDGE_CURVE('',#5996,#5984,#3329,.T.);
#7508=EDGE_CURVE('',#5994,#5996,#3330,.T.);
#7509=EDGE_CURVE('',#5980,#5997,#3331,.T.);
#7510=EDGE_CURVE('',#5998,#5997,#268,.T.);
#7511=EDGE_CURVE('',#5996,#5998,#269,.T.);
#7512=EDGE_CURVE('',#5999,#6000,#270,.T.);
#7513=EDGE_CURVE('',#5998,#6000,#271,.T.);
#7514=EDGE_CURVE('',#5997,#5999,#3332,.T.);
#7515=EDGE_CURVE('',#6001,#5995,#272,.T.);
#7516=EDGE_CURVE('',#6001,#5989,#273,.T.);
#7517=EDGE_CURVE('',#5994,#6002,#3333,.T.);
#7518=EDGE_CURVE('',#6002,#6001,#274,.T.);
#7519=EDGE_CURVE('',#5996,#6003,#3334,.T.);
#7520=EDGE_CURVE('',#6003,#6002,#3335,.T.);
#7521=EDGE_CURVE('',#6000,#6003,#275,.T.);
#7522=EDGE_CURVE('',#5990,#6004,#276,.T.);
#7523=EDGE_CURVE('',#6005,#6004,#277,.T.);
#7524=EDGE_CURVE('',#6005,#5991,#278,.T.);
#7525=EDGE_CURVE('',#6006,#6007,#279,.T.);
#7526=EDGE_CURVE('',#6008,#6007,#280,.T.);
#7527=EDGE_CURVE('',#6008,#6009,#281,.T.);
#7528=EDGE_CURVE('',#6009,#6006,#3336,.T.);
#7529=EDGE_CURVE('',#6007,#6010,#282,.T.);
#7530=EDGE_CURVE('',#6010,#6011,#3337,.T.);
#7531=EDGE_CURVE('',#6011,#6008,#283,.T.);
#7532=EDGE_CURVE('',#6010,#6012,#3338,.T.);
#7533=EDGE_CURVE('',#6012,#6013,#3339,.T.);
#7534=EDGE_CURVE('',#6013,#6011,#3340,.T.);
#7535=EDGE_CURVE('',#6004,#6013,#284,.T.);
#7536=EDGE_CURVE('',#6012,#6005,#285,.T.);
#7537=EDGE_CURVE('',#6012,#6014,#3341,.T.);
#7538=EDGE_CURVE('',#6015,#6014,#286,.T.);
#7539=EDGE_CURVE('',#5992,#6015,#287,.T.);
#7540=EDGE_CURVE('',#6016,#6010,#3342,.T.);
#7541=EDGE_CURVE('',#6014,#6016,#3343,.T.);
#7542=EDGE_CURVE('',#6006,#6017,#3344,.T.);
#7543=EDGE_CURVE('',#6018,#6017,#288,.T.);
#7544=EDGE_CURVE('',#6016,#6018,#289,.T.);
#7545=EDGE_CURVE('',#6019,#5983,#3345,.T.);
#7546=EDGE_CURVE('',#6017,#6019,#3346,.T.);
#7547=EDGE_CURVE('',#5999,#6009,#3347,.T.);
#7548=EDGE_CURVE('',#6020,#6015,#290,.T.);
#7549=EDGE_CURVE('',#6020,#5993,#291,.T.);
#7550=EDGE_CURVE('',#6019,#6021,#292,.T.);
#7551=EDGE_CURVE('',#6018,#6021,#293,.T.);
#7552=EDGE_CURVE('',#6021,#6022,#294,.T.);
#7553=EDGE_CURVE('',#6022,#6016,#3348,.T.);
#7554=EDGE_CURVE('',#6022,#6023,#3349,.T.);
#7555=EDGE_CURVE('',#6023,#6014,#3350,.T.);
#7556=EDGE_CURVE('',#6023,#6020,#295,.T.);
#7557=EDGE_CURVE('',#6023,#5987,#3351,.T.);
#7558=EDGE_CURVE('',#5985,#6022,#3352,.T.);
#7559=EDGE_CURVE('',#6011,#6003,#3353,.T.);
#7560=EDGE_CURVE('',#6002,#6013,#3354,.T.);
#7561=EDGE_CURVE('',#6024,#6025,#83,.F.);
#7562=EDGE_CURVE('',#6025,#6026,#951,.T.);
#7563=EDGE_CURVE('',#6026,#6027,#3355,.T.);
#7564=EDGE_CURVE('',#6027,#6024,#952,.T.);
#7565=EDGE_CURVE('',#6026,#6028,#3356,.T.);
#7566=EDGE_CURVE('',#6028,#6029,#3357,.T.);
#7567=EDGE_CURVE('',#6029,#6027,#3358,.T.);
#7568=EDGE_CURVE('',#6030,#6031,#84,.F.);
#7569=EDGE_CURVE('',#6031,#6029,#953,.T.);
#7570=EDGE_CURVE('',#6028,#6030,#954,.T.);
#7571=EDGE_CURVE('',#6032,#6030,#3359,.T.);
#7572=EDGE_CURVE('',#6028,#6033,#3360,.T.);
#7573=EDGE_CURVE('',#6034,#6033,#955,.T.);
#7574=EDGE_CURVE('',#6035,#6034,#3361,.T.);
#7575=EDGE_CURVE('',#6036,#6035,#956,.T.);
#7576=EDGE_CURVE('',#6032,#6036,#79,.F.);
#7577=EDGE_CURVE('',#6026,#6037,#3362,.T.);
#7578=EDGE_CURVE('',#6033,#6037,#3363,.T.);
#7579=EDGE_CURVE('',#6038,#6038,#957,.T.);
#7580=EDGE_CURVE('',#6025,#6039,#3364,.T.);
#7581=EDGE_CURVE('',#6039,#6040,#80,.T.);
#7582=EDGE_CURVE('',#6041,#6040,#958,.T.);
#7583=EDGE_CURVE('',#6041,#6042,#3365,.T.);
#7584=EDGE_CURVE('',#6037,#6042,#959,.T.);
#7585=EDGE_CURVE('',#6043,#6043,#960,.T.);
#7586=EDGE_CURVE('',#6043,#6044,#3366,.T.);
#7587=EDGE_CURVE('',#6044,#6044,#961,.T.);
#7588=EDGE_CURVE('',#6045,#6046,#962,.T.);
#7589=EDGE_CURVE('',#6047,#6045,#3367,.T.);
#7590=EDGE_CURVE('',#6048,#6047,#963,.T.);
#7591=EDGE_CURVE('',#6049,#6048,#3368,.T.);
#7592=EDGE_CURVE('',#6050,#6049,#964,.T.);
#7593=EDGE_CURVE('',#6051,#6050,#3369,.T.);
#7594=EDGE_CURVE('',#6052,#6051,#965,.T.);
#7595=EDGE_CURVE('',#6046,#6052,#3370,.T.);
#7596=EDGE_CURVE('',#6044,#6053,#3371,.T.);
#7597=EDGE_CURVE('',#6053,#6053,#966,.T.);
#7598=EDGE_CURVE('',#6054,#6055,#85,.F.);
#7599=EDGE_CURVE('',#6055,#6056,#967,.T.);
#7600=EDGE_CURVE('',#6056,#6057,#3372,.T.);
#7601=EDGE_CURVE('',#6057,#6054,#968,.T.);
#7602=EDGE_CURVE('',#6056,#6058,#3373,.T.);
#7603=EDGE_CURVE('',#6058,#6059,#3374,.T.);
#7604=EDGE_CURVE('',#6059,#6057,#3375,.T.);
#7605=EDGE_CURVE('',#6060,#6061,#86,.F.);
#7606=EDGE_CURVE('',#6061,#6059,#969,.T.);
#7607=EDGE_CURVE('',#6058,#6060,#970,.T.);
#7608=EDGE_CURVE('',#6062,#6060,#3376,.T.);
#7609=EDGE_CURVE('',#6058,#6063,#3377,.T.);
#7610=EDGE_CURVE('',#6064,#6063,#971,.T.);
#7611=EDGE_CURVE('',#6065,#6064,#3378,.T.);
#7612=EDGE_CURVE('',#6066,#6065,#972,.T.);
#7613=EDGE_CURVE('',#6062,#6066,#81,.F.);
#7614=EDGE_CURVE('',#6056,#6067,#3379,.T.);
#7615=EDGE_CURVE('',#6063,#6067,#3380,.T.);
#7616=EDGE_CURVE('',#6068,#6068,#973,.T.);
#7617=EDGE_CURVE('',#6055,#6069,#3381,.T.);
#7618=EDGE_CURVE('',#6069,#6070,#82,.T.);
#7619=EDGE_CURVE('',#6071,#6070,#974,.T.);
#7620=EDGE_CURVE('',#6071,#6072,#3382,.T.);
#7621=EDGE_CURVE('',#6067,#6072,#975,.T.);
#7622=EDGE_CURVE('',#6069,#6073,#3383,.T.);
#7623=EDGE_CURVE('',#6073,#6074,#3384,.T.);
#7624=EDGE_CURVE('',#6074,#6070,#3385,.T.);
#7625=EDGE_CURVE('',#6075,#6076,#3386,.T.);
#7626=EDGE_CURVE('',#6076,#6074,#976,.T.);
#7627=EDGE_CURVE('',#6073,#6075,#977,.T.);
#7628=EDGE_CURVE('',#6077,#6078,#3387,.T.);
#7629=EDGE_CURVE('',#6078,#6076,#3388,.T.);
#7630=EDGE_CURVE('',#6075,#6077,#3389,.T.);
#7631=EDGE_CURVE('',#6079,#6080,#3390,.T.);
#7632=EDGE_CURVE('',#6080,#6078,#978,.T.);
#7633=EDGE_CURVE('',#6077,#6079,#979,.T.);
#7634=EDGE_CURVE('',#6036,#6080,#3391,.T.);
#7635=EDGE_CURVE('',#6079,#6032,#3392,.T.);
#7636=EDGE_CURVE('',#6081,#6079,#3393,.T.);
#7637=EDGE_CURVE('',#6082,#6081,#3394,.T.);
#7638=EDGE_CURVE('',#6082,#6083,#3395,.T.);
#7639=EDGE_CURVE('',#6084,#6083,#3396,.T.);
#7640=EDGE_CURVE('',#6085,#6084,#3397,.T.);
#7641=EDGE_CURVE('',#6086,#6085,#3398,.T.);
#7642=EDGE_CURVE('',#6086,#6087,#3399,.T.);
#7643=EDGE_CURVE('',#6039,#6087,#3400,.T.);
#7644=EDGE_CURVE('',#6031,#6024,#3401,.T.);
#7645=EDGE_CURVE('',#6088,#6077,#3402,.T.);
#7646=EDGE_CURVE('',#6081,#6088,#980,.T.);
#7647=EDGE_CURVE('',#6089,#6075,#3403,.T.);
#7648=EDGE_CURVE('',#6088,#6089,#3404,.T.);
#7649=EDGE_CURVE('',#6090,#6073,#3405,.T.);
#7650=EDGE_CURVE('',#6089,#6090,#981,.T.);
#7651=EDGE_CURVE('',#6061,#6054,#3406,.T.);
#7652=EDGE_CURVE('',#6091,#6062,#3407,.T.);
#7653=EDGE_CURVE('',#6092,#6091,#3408,.T.);
#7654=EDGE_CURVE('',#6093,#6092,#3409,.T.);
#7655=EDGE_CURVE('',#6094,#6093,#3410,.T.);
#7656=EDGE_CURVE('',#6095,#6094,#3411,.T.);
#7657=EDGE_CURVE('',#6096,#6095,#3412,.T.);
#7658=EDGE_CURVE('',#6090,#6096,#3413,.T.);
#7659=EDGE_CURVE('',#6087,#6097,#3414,.T.);
#7660=EDGE_CURVE('',#6097,#6040,#3415,.T.);
#7661=EDGE_CURVE('',#6098,#6099,#3416,.T.);
#7662=EDGE_CURVE('',#6099,#6097,#982,.T.);
#7663=EDGE_CURVE('',#6087,#6098,#983,.T.);
#7664=EDGE_CURVE('',#6100,#6101,#3417,.T.);
#7665=EDGE_CURVE('',#6101,#6099,#3418,.T.);
#7666=EDGE_CURVE('',#6098,#6100,#3419,.T.);
#7667=EDGE_CURVE('',#6091,#6102,#3420,.T.);
#7668=EDGE_CURVE('',#6102,#6101,#984,.T.);
#7669=EDGE_CURVE('',#6100,#6091,#985,.T.);
#7670=EDGE_CURVE('',#6066,#6102,#3421,.T.);
#7671=EDGE_CURVE('',#6103,#6100,#3422,.T.);
#7672=EDGE_CURVE('',#6092,#6103,#986,.T.);
#7673=EDGE_CURVE('',#6104,#6098,#3423,.T.);
#7674=EDGE_CURVE('',#6103,#6104,#3424,.T.);
#7675=EDGE_CURVE('',#6104,#6086,#987,.T.);
#7676=EDGE_CURVE('',#6082,#6045,#3425,.T.);
#7677=EDGE_CURVE('',#6046,#6105,#3426,.T.);
#7678=EDGE_CURVE('',#6105,#6082,#988,.T.);
#7679=EDGE_CURVE('',#6081,#6047,#3427,.T.);
#7680=EDGE_CURVE('',#6088,#6048,#3428,.T.);
#7681=EDGE_CURVE('',#6089,#6049,#3429,.T.);
#7682=EDGE_CURVE('',#6090,#6050,#3430,.T.);
#7683=EDGE_CURVE('',#6096,#6051,#3431,.T.);
#7684=EDGE_CURVE('',#6106,#6052,#3432,.T.);
#7685=EDGE_CURVE('',#6096,#6106,#989,.T.);
#7686=EDGE_CURVE('',#6106,#6105,#3433,.T.);
#7687=EDGE_CURVE('',#6105,#6107,#3434,.T.);
#7688=EDGE_CURVE('',#6083,#6107,#990,.T.);
#7689=EDGE_CURVE('',#6093,#6108,#3435,.F.);
#7690=EDGE_CURVE('',#6108,#6109,#3436,.T.);
#7691=EDGE_CURVE('',#6109,#6094,#3437,.F.);
#7692=EDGE_CURVE('',#6110,#6108,#3438,.T.);
#7693=EDGE_CURVE('',#6111,#6110,#3439,.T.);
#7694=EDGE_CURVE('',#6109,#6111,#3440,.T.);
#7695=EDGE_CURVE('',#6084,#6111,#3441,.F.);
#7696=EDGE_CURVE('',#6110,#6085,#3442,.F.);
#7697=EDGE_CURVE('',#6033,#6112,#3443,.T.);
#7698=EDGE_CURVE('',#6112,#6113,#991,.T.);
#7699=EDGE_CURVE('',#6113,#6034,#3444,.T.);
#7700=EDGE_CURVE('',#6037,#6114,#3445,.T.);
#7701=EDGE_CURVE('',#6114,#6112,#3446,.T.);
#7702=EDGE_CURVE('',#6042,#6115,#3447,.T.);
#7703=EDGE_CURVE('',#6115,#6114,#992,.T.);
#7704=EDGE_CURVE('',#6064,#6116,#3448,.T.);
#7705=EDGE_CURVE('',#6116,#6115,#3449,.T.);
#7706=EDGE_CURVE('',#6042,#6064,#3450,.T.);
#7707=EDGE_CURVE('',#6063,#6117,#3451,.T.);
#7708=EDGE_CURVE('',#6117,#6116,#993,.T.);
#7709=EDGE_CURVE('',#6067,#6118,#3452,.T.);
#7710=EDGE_CURVE('',#6118,#6117,#3453,.T.);
#7711=EDGE_CURVE('',#6072,#6119,#3454,.T.);
#7712=EDGE_CURVE('',#6119,#6118,#994,.T.);
#7713=EDGE_CURVE('',#6113,#6119,#3455,.T.);
#7714=EDGE_CURVE('',#6072,#6034,#3456,.T.);
#7715=EDGE_CURVE('',#6065,#6041,#3457,.T.);
#7716=EDGE_CURVE('',#6120,#6121,#3458,.T.);
#7717=EDGE_CURVE('',#6122,#6120,#3459,.T.);
#7718=EDGE_CURVE('',#6123,#6122,#3460,.T.);
#7719=EDGE_CURVE('',#6121,#6123,#3461,.T.);
#7720=EDGE_CURVE('',#6124,#6125,#3462,.T.);
#7721=EDGE_CURVE('',#6126,#6124,#3463,.T.);
#7722=EDGE_CURVE('',#6127,#6126,#3464,.T.);
#7723=EDGE_CURVE('',#6125,#6127,#3465,.T.);
#7724=EDGE_CURVE('',#6128,#6129,#3466,.T.);
#7725=EDGE_CURVE('',#6130,#6128,#3467,.T.);
#7726=EDGE_CURVE('',#6131,#6130,#3468,.T.);
#7727=EDGE_CURVE('',#6129,#6131,#3469,.T.);
#7728=EDGE_CURVE('',#6132,#6133,#3470,.T.);
#7729=EDGE_CURVE('',#6134,#6132,#3471,.T.);
#7730=EDGE_CURVE('',#6135,#6134,#3472,.T.);
#7731=EDGE_CURVE('',#6133,#6135,#3473,.T.);
#7732=EDGE_CURVE('',#6109,#6136,#3474,.T.);
#7733=EDGE_CURVE('',#6136,#6095,#3475,.T.);
#7734=EDGE_CURVE('',#6137,#6138,#3476,.T.);
#7735=EDGE_CURVE('',#6138,#6095,#995,.T.);
#7736=EDGE_CURVE('',#6136,#6137,#996,.T.);
#7737=EDGE_CURVE('',#6139,#6107,#3477,.T.);
#7738=EDGE_CURVE('',#6107,#6138,#3478,.T.);
#7739=EDGE_CURVE('',#6137,#6139,#3479,.T.);
#7740=EDGE_CURVE('',#6140,#6083,#3480,.T.);
#7741=EDGE_CURVE('',#6139,#6140,#997,.T.);
#7742=EDGE_CURVE('',#6140,#6111,#3481,.T.);
#7743=EDGE_CURVE('',#6110,#6141,#3482,.T.);
#7744=EDGE_CURVE('',#6141,#6086,#3483,.T.);
#7745=EDGE_CURVE('',#6142,#6104,#3484,.T.);
#7746=EDGE_CURVE('',#6141,#6142,#998,.T.);
#7747=EDGE_CURVE('',#6143,#6103,#3485,.T.);
#7748=EDGE_CURVE('',#6142,#6143,#3486,.T.);
#7749=EDGE_CURVE('',#6144,#6092,#3487,.T.);
#7750=EDGE_CURVE('',#6143,#6144,#999,.T.);
#7751=EDGE_CURVE('',#6144,#6108,#3488,.T.);
#7752=EDGE_CURVE('',#6122,#6145,#3489,.T.);
#7753=EDGE_CURVE('',#6145,#6146,#3490,.T.);
#7754=EDGE_CURVE('',#6123,#6146,#3491,.T.);
#7755=EDGE_CURVE('',#6121,#6147,#3492,.T.);
#7756=EDGE_CURVE('',#6147,#6148,#3493,.T.);
#7757=EDGE_CURVE('',#6148,#6120,#3494,.T.);
#7758=EDGE_CURVE('',#6146,#6147,#3495,.T.);
#7759=EDGE_CURVE('',#6148,#6145,#3496,.T.);
#7760=EDGE_CURVE('',#6148,#6149,#3497,.T.);
#7761=EDGE_CURVE('',#6149,#6150,#3498,.T.);
#7762=EDGE_CURVE('',#6145,#6150,#3499,.T.);
#7763=EDGE_CURVE('',#6147,#6151,#3500,.T.);
#7764=EDGE_CURVE('',#6151,#6149,#3501,.T.);
#7765=EDGE_CURVE('',#6152,#6152,#1000,.T.);
#7766=EDGE_CURVE('',#6134,#6153,#3502,.T.);
#7767=EDGE_CURVE('',#6153,#6154,#3503,.T.);
#7768=EDGE_CURVE('',#6135,#6154,#3504,.T.);
#7769=EDGE_CURVE('',#6133,#6155,#3505,.T.);
#7770=EDGE_CURVE('',#6155,#6156,#3506,.T.);
#7771=EDGE_CURVE('',#6156,#6132,#3507,.T.);
#7772=EDGE_CURVE('',#6154,#6155,#3508,.T.);
#7773=EDGE_CURVE('',#6156,#6153,#3509,.T.);
#7774=EDGE_CURVE('',#6156,#6157,#3510,.T.);
#7775=EDGE_CURVE('',#6157,#6158,#3511,.T.);
#7776=EDGE_CURVE('',#6153,#6158,#3512,.T.);
#7777=EDGE_CURVE('',#6155,#6159,#3513,.T.);
#7778=EDGE_CURVE('',#6159,#6157,#3514,.T.);
#7779=EDGE_CURVE('',#6160,#6160,#1001,.T.);
#7780=EDGE_CURVE('',#6126,#6161,#3515,.T.);
#7781=EDGE_CURVE('',#6161,#6162,#3516,.T.);
#7782=EDGE_CURVE('',#6127,#6162,#3517,.T.);
#7783=EDGE_CURVE('',#6125,#6163,#3518,.T.);
#7784=EDGE_CURVE('',#6163,#6164,#3519,.T.);
#7785=EDGE_CURVE('',#6164,#6124,#3520,.T.);
#7786=EDGE_CURVE('',#6162,#6163,#3521,.T.);
#7787=EDGE_CURVE('',#6164,#6161,#3522,.T.);
#7788=EDGE_CURVE('',#6164,#6165,#3523,.T.);
#7789=EDGE_CURVE('',#6165,#6166,#3524,.T.);
#7790=EDGE_CURVE('',#6161,#6166,#3525,.T.);
#7791=EDGE_CURVE('',#6163,#6167,#3526,.T.);
#7792=EDGE_CURVE('',#6167,#6165,#3527,.T.);
#7793=EDGE_CURVE('',#6168,#6168,#1002,.T.);
#7794=EDGE_CURVE('',#6130,#6169,#3528,.T.);
#7795=EDGE_CURVE('',#6169,#6170,#3529,.T.);
#7796=EDGE_CURVE('',#6131,#6170,#3530,.T.);
#7797=EDGE_CURVE('',#6129,#6171,#3531,.T.);
#7798=EDGE_CURVE('',#6171,#6172,#3532,.T.);
#7799=EDGE_CURVE('',#6172,#6128,#3533,.T.);
#7800=EDGE_CURVE('',#6170,#6171,#3534,.T.);
#7801=EDGE_CURVE('',#6172,#6169,#3535,.T.);
#7802=EDGE_CURVE('',#6172,#6173,#3536,.T.);
#7803=EDGE_CURVE('',#6173,#6174,#3537,.T.);
#7804=EDGE_CURVE('',#6169,#6174,#3538,.T.);
#7805=EDGE_CURVE('',#6171,#6175,#3539,.T.);
#7806=EDGE_CURVE('',#6175,#6173,#3540,.T.);
#7807=EDGE_CURVE('',#6176,#6176,#1003,.T.);
#7808=EDGE_CURVE('',#6038,#6177,#3541,.T.);
#7809=EDGE_CURVE('',#6177,#6177,#1004,.T.);
#7810=EDGE_CURVE('',#6168,#6178,#3542,.T.);
#7811=EDGE_CURVE('',#6178,#6178,#1005,.T.);
#7812=EDGE_CURVE('',#6176,#6179,#3543,.T.);
#7813=EDGE_CURVE('',#6179,#6179,#1006,.T.);
#7814=EDGE_CURVE('',#6152,#6180,#3544,.T.);
#7815=EDGE_CURVE('',#6180,#6180,#1007,.T.);
#7816=EDGE_CURVE('',#6160,#6068,#3545,.T.);
#7817=EDGE_CURVE('',#6170,#6181,#3546,.T.);
#7818=EDGE_CURVE('',#6181,#6175,#3547,.T.);
#7819=EDGE_CURVE('',#6174,#6181,#3548,.T.);
#7820=EDGE_CURVE('',#6162,#6182,#3549,.T.);
#7821=EDGE_CURVE('',#6182,#6167,#3550,.T.);
#7822=EDGE_CURVE('',#6166,#6182,#3551,.T.);
#7823=EDGE_CURVE('',#6154,#6183,#3552,.T.);
#7824=EDGE_CURVE('',#6183,#6159,#3553,.T.);
#7825=EDGE_CURVE('',#6158,#6183,#3554,.T.);
#7826=EDGE_CURVE('',#6146,#6184,#3555,.T.);
#7827=EDGE_CURVE('',#6184,#6151,#3556,.T.);
#7828=EDGE_CURVE('',#6150,#6184,#3557,.T.);
#7829=EDGE_CURVE('',#6106,#6138,#3558,.T.);
#7830=EDGE_CURVE('',#6035,#6071,#3559,.T.);
#7831=EDGE_CURVE('',#6185,#6185,#1008,.T.);
#7832=EDGE_CURVE('',#6185,#6186,#3560,.T.);
#7833=EDGE_CURVE('',#6186,#6187,#1009,.T.);
#7834=EDGE_CURVE('',#6187,#6186,#1010,.T.);
#7835=EDGE_CURVE('',#6187,#6188,#3561,.T.);
#7836=EDGE_CURVE('',#6189,#6188,#1011,.T.);
#7837=EDGE_CURVE('',#6188,#6189,#1012,.T.);
#7838=EDGE_CURVE('',#6189,#6190,#3562,.T.);
#7839=EDGE_CURVE('',#6190,#6191,#1013,.T.);
#7840=EDGE_CURVE('',#6191,#6190,#1014,.T.);
#7841=EDGE_CURVE('',#6191,#6192,#3563,.T.);
#7842=EDGE_CURVE('',#6192,#6192,#1015,.T.);
#7843=EDGE_CURVE('',#6193,#6193,#1016,.T.);
#7844=EDGE_CURVE('',#6192,#6193,#3564,.T.);
#7845=EDGE_CURVE('',#6194,#6194,#1017,.T.);
#7846=EDGE_CURVE('',#6195,#6195,#1018,.T.);
#7847=EDGE_CURVE('',#6195,#6194,#3565,.T.);
#7848=EDGE_CURVE('',#6196,#6196,#1019,.T.);
#7849=EDGE_CURVE('',#6196,#6195,#3566,.T.);
#7850=EDGE_CURVE('',#6197,#6197,#1020,.T.);
#7851=EDGE_CURVE('',#6197,#6196,#3567,.T.);
#7852=EDGE_CURVE('',#6198,#6199,#3568,.T.);
#7853=EDGE_CURVE('',#6199,#6200,#3569,.T.);
#7854=EDGE_CURVE('',#6201,#6200,#3570,.T.);
#7855=EDGE_CURVE('',#6198,#6201,#3571,.T.);
#7856=EDGE_CURVE('',#6202,#6198,#3572,.T.);
#7857=EDGE_CURVE('',#6203,#6201,#3573,.T.);
#7858=EDGE_CURVE('',#6202,#6203,#3574,.T.);
#7859=EDGE_CURVE('',#6204,#6202,#3575,.T.);
#7860=EDGE_CURVE('',#6205,#6203,#3576,.T.);
#7861=EDGE_CURVE('',#6204,#6205,#3577,.T.);
#7862=EDGE_CURVE('',#6206,#6204,#3578,.T.);
#7863=EDGE_CURVE('',#6207,#6205,#3579,.T.);
#7864=EDGE_CURVE('',#6206,#6207,#3580,.T.);
#7865=EDGE_CURVE('',#6208,#6206,#3581,.T.);
#7866=EDGE_CURVE('',#6209,#6207,#3582,.T.);
#7867=EDGE_CURVE('',#6208,#6209,#3583,.T.);
#7868=EDGE_CURVE('',#6210,#6208,#3584,.T.);
#7869=EDGE_CURVE('',#6211,#6209,#3585,.T.);
#7870=EDGE_CURVE('',#6210,#6211,#3586,.T.);
#7871=EDGE_CURVE('',#6212,#6210,#3587,.T.);
#7872=EDGE_CURVE('',#6213,#6211,#3588,.T.);
#7873=EDGE_CURVE('',#6212,#6213,#3589,.T.);
#7874=EDGE_CURVE('',#6214,#6212,#3590,.T.);
#7875=EDGE_CURVE('',#6215,#6213,#3591,.T.);
#7876=EDGE_CURVE('',#6214,#6215,#3592,.T.);
#7877=EDGE_CURVE('',#6216,#6214,#3593,.T.);
#7878=EDGE_CURVE('',#6217,#6215,#3594,.T.);
#7879=EDGE_CURVE('',#6216,#6217,#3595,.T.);
#7880=EDGE_CURVE('',#6218,#6216,#3596,.T.);
#7881=EDGE_CURVE('',#6219,#6217,#3597,.T.);
#7882=EDGE_CURVE('',#6218,#6219,#3598,.T.);
#7883=EDGE_CURVE('',#6220,#6218,#3599,.T.);
#7884=EDGE_CURVE('',#6221,#6219,#3600,.T.);
#7885=EDGE_CURVE('',#6220,#6221,#3601,.T.);
#7886=EDGE_CURVE('',#6222,#6220,#3602,.T.);
#7887=EDGE_CURVE('',#6223,#6221,#3603,.T.);
#7888=EDGE_CURVE('',#6222,#6223,#3604,.T.);
#7889=EDGE_CURVE('',#6224,#6222,#3605,.T.);
#7890=EDGE_CURVE('',#6225,#6223,#3606,.T.);
#7891=EDGE_CURVE('',#6224,#6225,#3607,.T.);
#7892=EDGE_CURVE('',#6226,#6224,#3608,.T.);
#7893=EDGE_CURVE('',#6227,#6225,#3609,.T.);
#7894=EDGE_CURVE('',#6226,#6227,#3610,.T.);
#7895=EDGE_CURVE('',#6228,#6226,#3611,.T.);
#7896=EDGE_CURVE('',#6229,#6227,#3612,.T.);
#7897=EDGE_CURVE('',#6228,#6229,#3613,.T.);
#7898=EDGE_CURVE('',#6230,#6228,#3614,.T.);
#7899=EDGE_CURVE('',#6231,#6229,#3615,.T.);
#7900=EDGE_CURVE('',#6230,#6231,#3616,.T.);
#7901=EDGE_CURVE('',#6232,#6230,#3617,.T.);
#7902=EDGE_CURVE('',#6233,#6231,#3618,.T.);
#7903=EDGE_CURVE('',#6232,#6233,#3619,.T.);
#7904=EDGE_CURVE('',#6234,#6232,#3620,.T.);
#7905=EDGE_CURVE('',#6235,#6233,#3621,.T.);
#7906=EDGE_CURVE('',#6234,#6235,#3622,.T.);
#7907=EDGE_CURVE('',#6236,#6234,#3623,.T.);
#7908=EDGE_CURVE('',#6237,#6235,#3624,.T.);
#7909=EDGE_CURVE('',#6236,#6237,#3625,.T.);
#7910=EDGE_CURVE('',#6238,#6236,#3626,.T.);
#7911=EDGE_CURVE('',#6239,#6237,#3627,.T.);
#7912=EDGE_CURVE('',#6238,#6239,#3628,.T.);
#7913=EDGE_CURVE('',#6240,#6238,#3629,.T.);
#7914=EDGE_CURVE('',#6241,#6239,#3630,.T.);
#7915=EDGE_CURVE('',#6240,#6241,#3631,.T.);
#7916=EDGE_CURVE('',#6242,#6240,#3632,.T.);
#7917=EDGE_CURVE('',#6243,#6241,#3633,.T.);
#7918=EDGE_CURVE('',#6242,#6243,#3634,.T.);
#7919=EDGE_CURVE('',#6244,#6242,#3635,.T.);
#7920=EDGE_CURVE('',#6245,#6243,#3636,.T.);
#7921=EDGE_CURVE('',#6244,#6245,#3637,.T.);
#7922=EDGE_CURVE('',#6246,#6244,#3638,.T.);
#7923=EDGE_CURVE('',#6247,#6245,#3639,.T.);
#7924=EDGE_CURVE('',#6246,#6247,#3640,.T.);
#7925=EDGE_CURVE('',#6248,#6246,#3641,.T.);
#7926=EDGE_CURVE('',#6249,#6247,#3642,.T.);
#7927=EDGE_CURVE('',#6248,#6249,#3643,.T.);
#7928=EDGE_CURVE('',#6250,#6248,#3644,.T.);
#7929=EDGE_CURVE('',#6251,#6249,#3645,.T.);
#7930=EDGE_CURVE('',#6250,#6251,#3646,.T.);
#7931=EDGE_CURVE('',#6252,#6250,#3647,.T.);
#7932=EDGE_CURVE('',#6253,#6251,#3648,.T.);
#7933=EDGE_CURVE('',#6252,#6253,#3649,.T.);
#7934=EDGE_CURVE('',#6254,#6252,#3650,.T.);
#7935=EDGE_CURVE('',#6255,#6253,#3651,.T.);
#7936=EDGE_CURVE('',#6254,#6255,#3652,.T.);
#7937=EDGE_CURVE('',#6256,#6254,#3653,.T.);
#7938=EDGE_CURVE('',#6257,#6255,#3654,.T.);
#7939=EDGE_CURVE('',#6256,#6257,#3655,.T.);
#7940=EDGE_CURVE('',#6258,#6256,#3656,.T.);
#7941=EDGE_CURVE('',#6259,#6257,#3657,.T.);
#7942=EDGE_CURVE('',#6258,#6259,#3658,.T.);
#7943=EDGE_CURVE('',#6260,#6258,#3659,.T.);
#7944=EDGE_CURVE('',#6261,#6259,#3660,.T.);
#7945=EDGE_CURVE('',#6260,#6261,#3661,.T.);
#7946=EDGE_CURVE('',#6262,#6260,#3662,.T.);
#7947=EDGE_CURVE('',#6263,#6261,#3663,.T.);
#7948=EDGE_CURVE('',#6262,#6263,#3664,.T.);
#7949=EDGE_CURVE('',#6264,#6262,#3665,.T.);
#7950=EDGE_CURVE('',#6265,#6263,#3666,.T.);
#7951=EDGE_CURVE('',#6264,#6265,#3667,.T.);
#7952=EDGE_CURVE('',#6266,#6264,#3668,.T.);
#7953=EDGE_CURVE('',#6267,#6265,#3669,.T.);
#7954=EDGE_CURVE('',#6266,#6267,#3670,.T.);
#7955=EDGE_CURVE('',#6268,#6266,#3671,.T.);
#7956=EDGE_CURVE('',#6269,#6267,#3672,.T.);
#7957=EDGE_CURVE('',#6268,#6269,#3673,.T.);
#7958=EDGE_CURVE('',#6270,#6268,#3674,.T.);
#7959=EDGE_CURVE('',#6271,#6269,#3675,.T.);
#7960=EDGE_CURVE('',#6270,#6271,#3676,.T.);
#7961=EDGE_CURVE('',#6272,#6270,#3677,.T.);
#7962=EDGE_CURVE('',#6273,#6271,#3678,.T.);
#7963=EDGE_CURVE('',#6272,#6273,#3679,.T.);
#7964=EDGE_CURVE('',#6274,#6272,#3680,.T.);
#7965=EDGE_CURVE('',#6275,#6273,#3681,.T.);
#7966=EDGE_CURVE('',#6274,#6275,#3682,.T.);
#7967=EDGE_CURVE('',#6276,#6274,#3683,.T.);
#7968=EDGE_CURVE('',#6277,#6275,#3684,.T.);
#7969=EDGE_CURVE('',#6276,#6277,#3685,.T.);
#7970=EDGE_CURVE('',#6278,#6276,#3686,.T.);
#7971=EDGE_CURVE('',#6279,#6277,#3687,.T.);
#7972=EDGE_CURVE('',#6278,#6279,#3688,.T.);
#7973=EDGE_CURVE('',#6280,#6278,#3689,.T.);
#7974=EDGE_CURVE('',#6281,#6279,#3690,.T.);
#7975=EDGE_CURVE('',#6280,#6281,#3691,.T.);
#7976=EDGE_CURVE('',#6282,#6280,#3692,.T.);
#7977=EDGE_CURVE('',#6283,#6281,#3693,.T.);
#7978=EDGE_CURVE('',#6282,#6283,#3694,.T.);
#7979=EDGE_CURVE('',#6284,#6282,#3695,.T.);
#7980=EDGE_CURVE('',#6285,#6283,#3696,.T.);
#7981=EDGE_CURVE('',#6284,#6285,#3697,.T.);
#7982=EDGE_CURVE('',#6286,#6284,#3698,.T.);
#7983=EDGE_CURVE('',#6287,#6285,#3699,.T.);
#7984=EDGE_CURVE('',#6286,#6287,#3700,.T.);
#7985=EDGE_CURVE('',#6288,#6286,#3701,.T.);
#7986=EDGE_CURVE('',#6289,#6287,#3702,.T.);
#7987=EDGE_CURVE('',#6288,#6289,#3703,.T.);
#7988=EDGE_CURVE('',#6290,#6288,#3704,.T.);
#7989=EDGE_CURVE('',#6291,#6289,#3705,.T.);
#7990=EDGE_CURVE('',#6290,#6291,#3706,.T.);
#7991=EDGE_CURVE('',#6292,#6290,#3707,.T.);
#7992=EDGE_CURVE('',#6293,#6291,#3708,.T.);
#7993=EDGE_CURVE('',#6292,#6293,#3709,.T.);
#7994=EDGE_CURVE('',#6294,#6292,#3710,.T.);
#7995=EDGE_CURVE('',#6295,#6293,#3711,.T.);
#7996=EDGE_CURVE('',#6294,#6295,#3712,.T.);
#7997=EDGE_CURVE('',#6296,#6294,#3713,.T.);
#7998=EDGE_CURVE('',#6297,#6295,#3714,.T.);
#7999=EDGE_CURVE('',#6296,#6297,#3715,.T.);
#8000=EDGE_CURVE('',#6199,#6296,#3716,.T.);
#8001=EDGE_CURVE('',#6200,#6297,#3717,.T.);
#8002=EDGE_CURVE('',#6298,#6299,#3718,.T.);
#8003=EDGE_CURVE('',#6299,#6300,#3719,.T.);
#8004=EDGE_CURVE('',#6300,#6301,#3720,.T.);
#8005=EDGE_CURVE('',#6301,#6298,#3721,.T.);
#8006=EDGE_CURVE('',#6302,#6303,#3722,.T.);
#8007=EDGE_CURVE('',#6303,#6299,#1021,.T.);
#8008=EDGE_CURVE('',#6298,#6302,#1022,.T.);
#8009=EDGE_CURVE('',#6304,#6305,#3723,.T.);
#8010=EDGE_CURVE('',#6305,#6303,#3724,.T.);
#8011=EDGE_CURVE('',#6302,#6304,#3725,.T.);
#8012=EDGE_CURVE('',#6306,#6307,#3726,.T.);
#8013=EDGE_CURVE('',#6307,#6305,#1023,.T.);
#8014=EDGE_CURVE('',#6304,#6306,#1024,.T.);
#8015=EDGE_CURVE('',#6308,#6309,#3727,.T.);
#8016=EDGE_CURVE('',#6309,#6307,#3728,.T.);
#8017=EDGE_CURVE('',#6306,#6308,#3729,.T.);
#8018=EDGE_CURVE('',#6310,#6311,#3730,.T.);
#8019=EDGE_CURVE('',#6311,#6309,#1025,.T.);
#8020=EDGE_CURVE('',#6308,#6310,#1026,.T.);
#8021=EDGE_CURVE('',#6312,#6313,#3731,.T.);
#8022=EDGE_CURVE('',#6313,#6311,#3732,.T.);
#8023=EDGE_CURVE('',#6310,#6312,#3733,.T.);
#8024=EDGE_CURVE('',#6300,#6313,#1027,.T.);
#8025=EDGE_CURVE('',#6312,#6301,#1028,.T.);
#8026=EDGE_CURVE('',#6304,#6314,#3734,.T.);
#8027=EDGE_CURVE('',#6315,#6314,#1029,.T.);
#8028=EDGE_CURVE('',#6306,#6315,#3735,.T.);
#8029=EDGE_CURVE('',#6302,#6316,#3736,.T.);
#8030=EDGE_CURVE('',#6314,#6316,#3737,.T.);
#8031=EDGE_CURVE('',#6298,#6317,#3738,.T.);
#8032=EDGE_CURVE('',#6316,#6317,#1030,.T.);
#8033=EDGE_CURVE('',#6301,#6318,#3739,.T.);
#8034=EDGE_CURVE('',#6317,#6318,#3740,.T.);
#8035=EDGE_CURVE('',#6319,#6320,#3741,.T.);
#8036=EDGE_CURVE('',#6321,#6319,#1031,.T.);
#8037=EDGE_CURVE('',#6322,#6321,#3742,.T.);
#8038=EDGE_CURVE('',#6323,#6322,#1032,.T.);
#8039=EDGE_CURVE('',#6324,#6323,#3743,.T.);
#8040=EDGE_CURVE('',#6325,#6324,#1033,.T.);
#8041=EDGE_CURVE('',#6326,#6325,#3744,.T.);
#8042=EDGE_CURVE('',#6320,#6326,#1034,.T.);
#8043=EDGE_CURVE('',#6327,#6328,#3745,.T.);
#8044=EDGE_CURVE('',#6328,#6329,#1035,.T.);
#8045=EDGE_CURVE('',#6329,#6330,#3746,.T.);
#8046=EDGE_CURVE('',#6330,#6327,#1036,.T.);
#8047=EDGE_CURVE('',#6331,#6332,#3747,.T.);
#8048=EDGE_CURVE('',#6332,#6328,#3748,.T.);
#8049=EDGE_CURVE('',#6327,#6331,#3749,.T.);
#8050=EDGE_CURVE('',#6333,#6334,#3750,.T.);
#8051=EDGE_CURVE('',#6334,#6332,#1037,.T.);
#8052=EDGE_CURVE('',#6331,#6333,#1038,.T.);
#8053=EDGE_CURVE('',#6335,#6336,#3751,.T.);
#8054=EDGE_CURVE('',#6336,#6334,#3752,.T.);
#8055=EDGE_CURVE('',#6333,#6335,#3753,.T.);
#8056=EDGE_CURVE('',#6337,#6338,#3754,.T.);
#8057=EDGE_CURVE('',#6338,#6336,#1039,.T.);
#8058=EDGE_CURVE('',#6335,#6337,#1040,.T.);
#8059=EDGE_CURVE('',#6339,#6340,#3755,.T.);
#8060=EDGE_CURVE('',#6340,#6338,#3756,.T.);
#8061=EDGE_CURVE('',#6337,#6339,#3757,.T.);
#8062=EDGE_CURVE('',#6341,#6342,#3758,.T.);
#8063=EDGE_CURVE('',#6342,#6340,#1041,.T.);
#8064=EDGE_CURVE('',#6339,#6341,#1042,.T.);
#8065=EDGE_CURVE('',#6329,#6342,#3759,.T.);
#8066=EDGE_CURVE('',#6341,#6330,#3760,.T.);
#8067=EDGE_CURVE('',#6333,#6326,#3761,.T.);
#8068=EDGE_CURVE('',#6335,#6325,#3762,.T.);
#8069=EDGE_CURVE('',#6331,#6320,#3763,.T.);
#8070=EDGE_CURVE('',#6327,#6319,#3764,.T.);
#8071=EDGE_CURVE('',#6330,#6321,#3765,.T.);
#8072=EDGE_CURVE('',#6343,#6344,#1043,.T.);
#8073=EDGE_CURVE('',#6345,#6343,#3766,.T.);
#8074=EDGE_CURVE('',#6346,#6345,#1044,.T.);
#8075=EDGE_CURVE('',#6347,#6346,#3767,.T.);
#8076=EDGE_CURVE('',#6348,#6347,#1045,.T.);
#8077=EDGE_CURVE('',#6349,#6348,#3768,.T.);
#8078=EDGE_CURVE('',#6350,#6349,#1046,.T.);
#8079=EDGE_CURVE('',#6344,#6350,#3769,.T.);
#8080=EDGE_CURVE('',#6351,#6343,#3770,.T.);
#8081=EDGE_CURVE('',#6344,#6352,#3771,.T.);
#8082=EDGE_CURVE('',#6352,#6351,#1047,.T.);
#8083=EDGE_CURVE('',#6351,#6353,#3772,.T.);
#8084=EDGE_CURVE('',#6353,#6345,#3773,.T.);
#8085=EDGE_CURVE('',#6354,#6346,#3774,.T.);
#8086=EDGE_CURVE('',#6353,#6354,#1048,.T.);
#8087=EDGE_CURVE('',#6354,#6355,#3775,.T.);
#8088=EDGE_CURVE('',#6355,#6347,#3776,.T.);
#8089=EDGE_CURVE('',#6356,#6348,#3777,.T.);
#8090=EDGE_CURVE('',#6355,#6356,#1049,.T.);
#8091=EDGE_CURVE('',#6356,#6357,#3778,.T.);
#8092=EDGE_CURVE('',#6357,#6349,#3779,.T.);
#8093=EDGE_CURVE('',#6358,#6350,#3780,.T.);
#8094=EDGE_CURVE('',#6357,#6358,#1050,.T.);
#8095=EDGE_CURVE('',#6358,#6352,#3781,.T.);
#8096=EDGE_CURVE('',#6354,#6359,#3782,.T.);
#8097=EDGE_CURVE('',#6360,#6359,#3783,.T.);
#8098=EDGE_CURVE('',#6361,#6360,#3784,.T.);
#8099=EDGE_CURVE('',#6362,#6361,#3785,.T.);
#8100=EDGE_CURVE('',#6355,#6362,#3786,.T.);
#8101=EDGE_CURVE('',#6353,#6363,#3787,.T.);
#8102=EDGE_CURVE('',#6364,#6363,#296,.T.);
#8103=EDGE_CURVE('',#6365,#6364,#297,.T.);
#8104=EDGE_CURVE('',#6366,#6365,#298,.T.);
#8105=EDGE_CURVE('',#6367,#6366,#1051,.T.);
#8106=EDGE_CURVE('',#6368,#6367,#299,.T.);
#8107=EDGE_CURVE('',#6369,#6368,#300,.T.);
#8108=EDGE_CURVE('',#6359,#6369,#301,.T.);
#8109=EDGE_CURVE('',#6351,#6370,#3788,.T.);
#8110=EDGE_CURVE('',#6371,#6370,#3789,.T.);
#8111=EDGE_CURVE('',#6372,#6371,#3790,.T.);
#8112=EDGE_CURVE('',#6363,#6372,#3791,.T.);
#8113=EDGE_CURVE('',#6352,#6373,#3792,.T.);
#8114=EDGE_CURVE('',#6374,#6373,#302,.T.);
#8115=EDGE_CURVE('',#6375,#6374,#303,.T.);
#8116=EDGE_CURVE('',#6376,#6375,#304,.T.);
#8117=EDGE_CURVE('',#6377,#6376,#1052,.T.);
#8118=EDGE_CURVE('',#6378,#6377,#305,.T.);
#8119=EDGE_CURVE('',#6379,#6378,#306,.T.);
#8120=EDGE_CURVE('',#6370,#6379,#307,.T.);
#8121=EDGE_CURVE('',#6361,#6380,#308,.T.);
#8122=EDGE_CURVE('',#6381,#6380,#309,.T.);
#8123=EDGE_CURVE('',#6381,#6362,#310,.T.);
#8124=EDGE_CURVE('',#6382,#6383,#311,.T.);
#8125=EDGE_CURVE('',#6384,#6383,#312,.T.);
#8126=EDGE_CURVE('',#6384,#6385,#313,.T.);
#8127=EDGE_CURVE('',#6385,#6382,#3793,.T.);
#8128=EDGE_CURVE('',#6383,#6386,#314,.T.);
#8129=EDGE_CURVE('',#6386,#6387,#3794,.T.);
#8130=EDGE_CURVE('',#6387,#6384,#315,.T.);
#8131=EDGE_CURVE('',#6388,#6389,#3795,.T.);
#8132=EDGE_CURVE('',#6389,#6390,#1053,.T.);
#8133=EDGE_CURVE('',#6390,#6391,#3796,.T.);
#8134=EDGE_CURVE('',#6391,#6388,#1054,.T.);
#8135=EDGE_CURVE('',#6390,#6387,#316,.T.);
#8136=EDGE_CURVE('',#6386,#6391,#317,.T.);
#8137=EDGE_CURVE('',#6380,#6392,#318,.T.);
#8138=EDGE_CURVE('',#6392,#6393,#3797,.T.);
#8139=EDGE_CURVE('',#6393,#6381,#319,.T.);
#8140=EDGE_CURVE('',#6392,#6389,#320,.T.);
#8141=EDGE_CURVE('',#6388,#6393,#321,.T.);
#8142=EDGE_CURVE('',#6394,#6360,#322,.T.);
#8143=EDGE_CURVE('',#6395,#6394,#323,.T.);
#8144=EDGE_CURVE('',#6395,#6392,#3798,.T.);
#8145=EDGE_CURVE('',#6356,#6382,#3799,.T.);
#8146=EDGE_CURVE('',#6396,#6397,#324,.T.);
#8147=EDGE_CURVE('',#6398,#6397,#325,.T.);
#8148=EDGE_CURVE('',#6398,#6399,#326,.T.);
#8149=EDGE_CURVE('',#6399,#6396,#3800,.T.);
#8150=EDGE_CURVE('',#6400,#6401,#327,.T.);
#8151=EDGE_CURVE('',#6402,#6401,#328,.T.);
#8152=EDGE_CURVE('',#6402,#6403,#329,.T.);
#8153=EDGE_CURVE('',#6403,#6400,#3801,.T.);
#8154=EDGE_CURVE('',#6401,#6404,#330,.T.);
#8155=EDGE_CURVE('',#6404,#6405,#3802,.T.);
#8156=EDGE_CURVE('',#6405,#6402,#331,.T.);
#8157=EDGE_CURVE('',#6406,#6407,#3803,.T.);
#8158=EDGE_CURVE('',#6407,#6408,#1055,.T.);
#8159=EDGE_CURVE('',#6408,#6409,#3804,.T.);
#8160=EDGE_CURVE('',#6409,#6406,#1056,.T.);
#8161=EDGE_CURVE('',#6408,#6405,#332,.T.);
#8162=EDGE_CURVE('',#6404,#6409,#333,.T.);
#8163=EDGE_CURVE('',#6397,#6410,#334,.T.);
#8164=EDGE_CURVE('',#6410,#6411,#3805,.T.);
#8165=EDGE_CURVE('',#6411,#6398,#335,.T.);
#8166=EDGE_CURVE('',#6410,#6407,#336,.T.);
#8167=EDGE_CURVE('',#6406,#6411,#337,.T.);
#8168=EDGE_CURVE('',#6387,#6410,#3806,.T.);
#8169=EDGE_CURVE('',#6396,#6385,#3807,.T.);
#8170=EDGE_CURVE('',#6357,#6399,#3808,.T.);
#8171=EDGE_CURVE('',#6358,#6400,#3809,.T.);
#8172=EDGE_CURVE('',#6314,#6412,#3810,.T.);
#8173=EDGE_CURVE('',#6412,#6413,#1057,.T.);
#8174=EDGE_CURVE('',#6413,#6315,#3811,.T.);
#8175=EDGE_CURVE('',#6316,#6414,#3812,.T.);
#8176=EDGE_CURVE('',#6414,#6412,#3813,.T.);
#8177=EDGE_CURVE('',#6317,#6415,#3814,.T.);
#8178=EDGE_CURVE('',#6415,#6414,#1058,.T.);
#8179=EDGE_CURVE('',#6318,#6416,#3815,.T.);
#8180=EDGE_CURVE('',#6416,#6415,#3816,.T.);
#8181=EDGE_CURVE('',#6417,#6418,#3817,.T.);
#8182=EDGE_CURVE('',#6418,#6416,#1059,.T.);
#8183=EDGE_CURVE('',#6318,#6417,#1060,.T.);
#8184=EDGE_CURVE('',#6419,#6420,#3818,.T.);
#8185=EDGE_CURVE('',#6420,#6418,#3819,.T.);
#8186=EDGE_CURVE('',#6417,#6419,#3820,.T.);
#8187=EDGE_CURVE('',#6421,#6422,#3821,.T.);
#8188=EDGE_CURVE('',#6422,#6420,#1061,.T.);
#8189=EDGE_CURVE('',#6419,#6421,#1062,.T.);
#8190=EDGE_CURVE('',#6413,#6422,#3822,.T.);
#8191=EDGE_CURVE('',#6421,#6315,#3823,.T.);
#8192=EDGE_CURVE('',#6423,#6395,#338,.T.);
#8193=EDGE_CURVE('',#6424,#6423,#1063,.T.);
#8194=EDGE_CURVE('',#6425,#6424,#339,.T.);
#8195=EDGE_CURVE('',#6426,#6425,#3824,.T.);
#8196=EDGE_CURVE('',#6427,#6426,#340,.T.);
#8197=EDGE_CURVE('',#6428,#6427,#1064,.T.);
#8198=EDGE_CURVE('',#6429,#6428,#341,.T.);
#8199=EDGE_CURVE('',#6405,#6429,#3825,.T.);
#8200=EDGE_CURVE('',#6372,#6430,#342,.T.);
#8201=EDGE_CURVE('',#6364,#6430,#343,.T.);
#8202=EDGE_CURVE('',#6394,#6369,#344,.T.);
#8203=EDGE_CURVE('',#6368,#6395,#3826,.T.);
#8204=EDGE_CURVE('',#6366,#6424,#3827,.T.);
#8205=EDGE_CURVE('',#6423,#6367,#3828,.T.);
#8206=EDGE_CURVE('',#6430,#6425,#345,.T.);
#8207=EDGE_CURVE('',#6425,#6365,#3829,.T.);
#8208=EDGE_CURVE('',#6431,#6371,#346,.T.);
#8209=EDGE_CURVE('',#6426,#6431,#347,.T.);
#8210=EDGE_CURVE('',#6432,#6433,#348,.T.);
#8211=EDGE_CURVE('',#6374,#6433,#349,.T.);
#8212=EDGE_CURVE('',#6373,#6432,#3830,.T.);
#8213=EDGE_CURVE('',#6431,#6379,#350,.T.);
#8214=EDGE_CURVE('',#6378,#6426,#3831,.T.);
#8215=EDGE_CURVE('',#6376,#6428,#3832,.T.);
#8216=EDGE_CURVE('',#6427,#6377,#3833,.T.);
#8217=EDGE_CURVE('',#6433,#6429,#351,.T.);
#8218=EDGE_CURVE('',#6429,#6375,#3834,.T.);
#8219=EDGE_CURVE('',#6432,#6403,#3835,.T.);
#8220=EDGE_CURVE('',#6308,#6421,#3836,.T.);
#8221=EDGE_CURVE('',#6310,#6419,#3837,.T.);
#8222=EDGE_CURVE('',#6312,#6417,#3838,.T.);
#8223=EDGE_CURVE('',#6337,#6324,#3839,.T.);
#8224=EDGE_CURVE('',#6339,#6323,#3840,.T.);
#8225=EDGE_CURVE('',#6341,#6322,#3841,.T.);
#8226=EDGE_CURVE('',#6434,#6435,#3842,.T.);
#8227=EDGE_CURVE('',#6435,#6436,#3843,.T.);
#8228=EDGE_CURVE('',#6436,#6437,#3844,.T.);
#8229=EDGE_CURVE('',#6437,#6438,#3845,.T.);
#8230=EDGE_CURVE('',#6438,#6439,#3846,.T.);
#8231=EDGE_CURVE('',#6439,#6434,#3847,.T.);
#8232=EDGE_CURVE('',#6440,#6441,#3848,.T.);
#8233=EDGE_CURVE('',#6441,#6435,#1065,.T.);
#8234=EDGE_CURVE('',#6434,#6440,#1066,.T.);
#8235=EDGE_CURVE('',#6442,#6443,#3849,.T.);
#8236=EDGE_CURVE('',#6443,#6441,#3850,.T.);
#8237=EDGE_CURVE('',#6440,#6442,#3851,.T.);
#8238=EDGE_CURVE('',#6444,#6445,#3852,.T.);
#8239=EDGE_CURVE('',#6445,#6443,#1067,.T.);
#8240=EDGE_CURVE('',#6442,#6444,#1068,.T.);
#8241=EDGE_CURVE('',#6446,#6447,#3853,.T.);
#8242=EDGE_CURVE('',#6447,#6445,#3854,.T.);
#8243=EDGE_CURVE('',#6444,#6446,#3855,.T.);
#8244=EDGE_CURVE('',#6448,#6449,#3856,.T.);
#8245=EDGE_CURVE('',#6449,#6447,#1069,.T.);
#8246=EDGE_CURVE('',#6446,#6448,#1070,.T.);
#8247=EDGE_CURVE('',#6450,#6451,#3857,.T.);
#8248=EDGE_CURVE('',#6451,#6449,#3858,.T.);
#8249=EDGE_CURVE('',#6448,#6450,#3859,.T.);
#8250=EDGE_CURVE('',#6438,#6451,#1071,.T.);
#8251=EDGE_CURVE('',#6450,#6439,#1072,.T.);
#8252=EDGE_CURVE('',#6452,#6437,#3860,.F.);
#8253=EDGE_CURVE('',#6452,#6453,#3861,.T.);
#8254=EDGE_CURVE('',#6454,#6453,#3862,.T.);
#8255=EDGE_CURVE('',#6455,#6454,#1073,.T.);
#8256=EDGE_CURVE('',#6456,#6455,#3863,.T.);
#8257=EDGE_CURVE('',#6457,#6456,#1074,.T.);
#8258=EDGE_CURVE('',#6458,#6457,#3864,.T.);
#8259=EDGE_CURVE('',#6459,#6458,#1075,.T.);
#8260=EDGE_CURVE('',#6460,#6459,#3865,.T.);
#8261=EDGE_CURVE('',#6461,#6460,#1076,.T.);
#8262=EDGE_CURVE('',#6462,#6461,#3866,.T.);
#8263=EDGE_CURVE('',#6462,#6463,#3867,.T.);
#8264=EDGE_CURVE('',#6436,#6463,#3868,.F.);
#8265=EDGE_CURVE('',#6442,#6464,#3869,.T.);
#8266=EDGE_CURVE('',#6464,#6465,#1077,.T.);
#8267=EDGE_CURVE('',#6444,#6465,#3870,.T.);
#8268=EDGE_CURVE('',#6440,#6466,#3871,.T.);
#8269=EDGE_CURVE('',#6466,#6464,#3872,.T.);
#8270=EDGE_CURVE('',#6434,#6467,#3873,.T.);
#8271=EDGE_CURVE('',#6467,#6466,#1078,.T.);
#8272=EDGE_CURVE('',#6439,#6468,#3874,.T.);
#8273=EDGE_CURVE('',#6468,#6467,#3875,.T.);
#8274=EDGE_CURVE('',#6469,#6470,#3876,.T.);
#8275=EDGE_CURVE('',#6471,#6469,#3877,.T.);
#8276=EDGE_CURVE('',#6470,#6471,#3878,.T.);
#8277=EDGE_CURVE('',#6472,#6473,#3879,.T.);
#8278=EDGE_CURVE('',#6473,#6471,#3880,.T.);
#8279=EDGE_CURVE('',#6469,#6474,#3881,.T.);
#8280=EDGE_CURVE('',#6474,#6472,#3882,.T.);
#8281=EDGE_CURVE('',#6475,#6476,#3883,.T.);
#8282=EDGE_CURVE('',#6476,#6470,#3884,.T.);
#8283=EDGE_CURVE('',#6471,#6477,#3885,.T.);
#8284=EDGE_CURVE('',#6477,#6475,#3886,.T.);
#8285=EDGE_CURVE('',#6437,#6469,#3887,.T.);
#8286=EDGE_CURVE('',#6470,#6452,#3888,.T.);
#8287=EDGE_CURVE('',#6478,#6473,#3889,.T.);
#8288=EDGE_CURVE('',#6477,#6478,#3890,.T.);
#8289=EDGE_CURVE('',#6479,#6472,#3891,.T.);
#8290=EDGE_CURVE('',#6479,#6480,#3892,.T.);
#8291=EDGE_CURVE('',#6480,#6478,#3893,.T.);
#8292=EDGE_CURVE('',#6474,#6436,#3894,.T.);
#8293=EDGE_CURVE('',#6463,#6479,#3895,.T.);
#8294=EDGE_CURVE('',#6481,#6482,#352,.T.);
#8295=EDGE_CURVE('',#6483,#6482,#353,.T.);
#8296=EDGE_CURVE('',#6483,#6484,#354,.T.);
#8297=EDGE_CURVE('',#6484,#6481,#3896,.T.);
#8298=EDGE_CURVE('',#6485,#6486,#355,.T.);
#8299=EDGE_CURVE('',#6487,#6486,#356,.T.);
#8300=EDGE_CURVE('',#6487,#6488,#357,.T.);
#8301=EDGE_CURVE('',#6488,#6485,#3897,.T.);
#8302=EDGE_CURVE('',#6486,#6489,#358,.T.);
#8303=EDGE_CURVE('',#6489,#6490,#3898,.T.);
#8304=EDGE_CURVE('',#6490,#6487,#359,.T.);
#8305=EDGE_CURVE('',#6491,#6492,#3899,.T.);
#8306=EDGE_CURVE('',#6492,#6493,#1079,.T.);
#8307=EDGE_CURVE('',#6493,#6494,#3900,.T.);
#8308=EDGE_CURVE('',#6494,#6491,#1080,.T.);
#8309=EDGE_CURVE('',#6491,#6490,#360,.T.);
#8310=EDGE_CURVE('',#6489,#6492,#361,.T.);
#8311=EDGE_CURVE('',#6482,#6495,#362,.T.);
#8312=EDGE_CURVE('',#6495,#6496,#3901,.T.);
#8313=EDGE_CURVE('',#6496,#6483,#363,.T.);
#8314=EDGE_CURVE('',#6495,#6494,#364,.T.);
#8315=EDGE_CURVE('',#6493,#6496,#365,.T.);
#8316=EDGE_CURVE('',#6481,#6497,#3902,.T.);
#8317=EDGE_CURVE('',#6498,#6497,#366,.T.);
#8318=EDGE_CURVE('',#6499,#6498,#367,.T.);
#8319=EDGE_CURVE('',#6499,#6495,#3903,.T.);
#8320=EDGE_CURVE('',#6484,#6500,#3904,.T.);
#8321=EDGE_CURVE('',#6501,#6500,#3905,.T.);
#8322=EDGE_CURVE('',#6502,#6501,#3906,.T.);
#8323=EDGE_CURVE('',#6497,#6502,#3907,.T.);
#8324=EDGE_CURVE('',#6485,#6503,#3908,.T.);
#8325=EDGE_CURVE('',#6500,#6503,#1081,.T.);
#8326=EDGE_CURVE('',#6504,#6505,#368,.T.);
#8327=EDGE_CURVE('',#6506,#6505,#369,.T.);
#8328=EDGE_CURVE('',#6506,#6507,#370,.T.);
#8329=EDGE_CURVE('',#6507,#6504,#3909,.T.);
#8330=EDGE_CURVE('',#6502,#6508,#371,.T.);
#8331=EDGE_CURVE('',#6498,#6508,#372,.T.);
#8332=EDGE_CURVE('',#6508,#6509,#373,.T.);
#8333=EDGE_CURVE('',#6509,#6499,#3910,.T.);
#8334=EDGE_CURVE('',#6510,#6511,#3911,.T.);
#8335=EDGE_CURVE('',#6511,#6512,#1082,.T.);
#8336=EDGE_CURVE('',#6512,#6513,#3912,.T.);
#8337=EDGE_CURVE('',#6513,#6510,#1083,.T.);
#8338=EDGE_CURVE('',#6510,#6499,#374,.T.);
#8339=EDGE_CURVE('',#6509,#6511,#375,.T.);
#8340=EDGE_CURVE('',#6505,#6514,#376,.T.);
#8341=EDGE_CURVE('',#6514,#6515,#3913,.T.);
#8342=EDGE_CURVE('',#6515,#6506,#377,.T.);
#8343=EDGE_CURVE('',#6514,#6513,#378,.T.);
#8344=EDGE_CURVE('',#6512,#6515,#379,.T.);
#8345=EDGE_CURVE('',#6516,#6514,#3914,.T.);
#8346=EDGE_CURVE('',#6517,#6516,#380,.T.);
#8347=EDGE_CURVE('',#6518,#6517,#1084,.T.);
#8348=EDGE_CURVE('',#6519,#6518,#381,.T.);
#8349=EDGE_CURVE('',#6520,#6519,#3915,.T.);
#8350=EDGE_CURVE('',#6521,#6520,#382,.T.);
#8351=EDGE_CURVE('',#6522,#6521,#1085,.T.);
#8352=EDGE_CURVE('',#6523,#6522,#383,.T.);
#8353=EDGE_CURVE('',#6490,#6523,#3916,.T.);
#8354=EDGE_CURVE('',#6478,#6524,#3917,.T.);
#8355=EDGE_CURVE('',#6524,#6480,#3918,.T.);
#8356=EDGE_CURVE('',#6524,#6525,#3919,.T.);
#8357=EDGE_CURVE('',#6525,#6475,#3920,.T.);
#8358=EDGE_CURVE('',#6526,#6527,#3921,.T.);
#8359=EDGE_CURVE('',#6527,#6454,#3922,.T.);
#8360=EDGE_CURVE('',#6453,#6526,#3923,.T.);
#8361=EDGE_CURVE('',#6528,#6455,#3924,.T.);
#8362=EDGE_CURVE('',#6527,#6528,#1086,.T.);
#8363=EDGE_CURVE('',#6529,#6456,#3925,.T.);
#8364=EDGE_CURVE('',#6528,#6529,#3926,.T.);
#8365=EDGE_CURVE('',#6501,#6457,#3927,.T.);
#8366=EDGE_CURVE('',#6529,#6501,#1087,.T.);
#8367=EDGE_CURVE('',#6500,#6458,#3928,.T.);
#8368=EDGE_CURVE('',#6503,#6459,#3929,.T.);
#8369=EDGE_CURVE('',#6530,#6460,#3930,.T.);
#8370=EDGE_CURVE('',#6503,#6530,#3931,.T.);
#8371=EDGE_CURVE('',#6531,#6461,#3932,.T.);
#8372=EDGE_CURVE('',#6530,#6531,#1088,.T.);
#8373=EDGE_CURVE('',#6531,#6532,#3933,.T.);
#8374=EDGE_CURVE('',#6532,#6462,#3934,.T.);
#8375=EDGE_CURVE('',#6525,#6526,#3935,.T.);
#8376=EDGE_CURVE('',#6453,#6476,#3936,.T.);
#8377=EDGE_CURVE('',#6532,#6524,#3937,.T.);
#8378=EDGE_CURVE('',#6480,#6462,#3938,.T.);
#8379=EDGE_CURVE('',#6507,#6529,#3939,.T.);
#8380=EDGE_CURVE('',#6533,#6528,#3940,.T.);
#8381=EDGE_CURVE('',#6534,#6533,#3941,.T.);
#8382=EDGE_CURVE('',#6504,#6534,#3942,.T.);
#8383=EDGE_CURVE('',#6535,#6527,#3943,.T.);
#8384=EDGE_CURVE('',#6536,#6535,#384,.T.);
#8385=EDGE_CURVE('',#6537,#6536,#385,.T.);
#8386=EDGE_CURVE('',#6538,#6537,#386,.T.);
#8387=EDGE_CURVE('',#6539,#6538,#1089,.T.);
#8388=EDGE_CURVE('',#6540,#6539,#387,.T.);
#8389=EDGE_CURVE('',#6541,#6540,#87,.T.);
#8390=EDGE_CURVE('',#6533,#6541,#388,.T.);
#8391=EDGE_CURVE('',#6542,#6543,#389,.T.);
#8392=EDGE_CURVE('',#6544,#6543,#390,.T.);
#8393=EDGE_CURVE('',#6544,#6545,#391,.T.);
#8394=EDGE_CURVE('',#6545,#6542,#3944,.T.);
#8395=EDGE_CURVE('',#6546,#6547,#392,.T.);
#8396=EDGE_CURVE('',#6548,#6547,#393,.T.);
#8397=EDGE_CURVE('',#6548,#6549,#394,.T.);
#8398=EDGE_CURVE('',#6549,#6546,#3945,.T.);
#8399=EDGE_CURVE('',#6547,#6550,#395,.T.);
#8400=EDGE_CURVE('',#6550,#6520,#3946,.T.);
#8401=EDGE_CURVE('',#6520,#6548,#396,.T.);
#8402=EDGE_CURVE('',#6521,#6551,#3947,.T.);
#8403=EDGE_CURVE('',#6551,#6552,#1090,.T.);
#8404=EDGE_CURVE('',#6552,#6522,#3948,.T.);
#8405=EDGE_CURVE('',#6550,#6551,#397,.T.);
#8406=EDGE_CURVE('',#6543,#6523,#398,.T.);
#8407=EDGE_CURVE('',#6523,#6553,#3949,.T.);
#8408=EDGE_CURVE('',#6553,#6544,#399,.T.);
#8409=EDGE_CURVE('',#6552,#6553,#400,.T.);
#8410=EDGE_CURVE('',#6542,#6488,#3950,.T.);
#8411=EDGE_CURVE('',#6545,#6530,#3951,.T.);
#8412=EDGE_CURVE('',#6546,#6531,#3952,.T.);
#8413=EDGE_CURVE('',#6554,#6555,#401,.T.);
#8414=EDGE_CURVE('',#6536,#6555,#402,.T.);
#8415=EDGE_CURVE('',#6535,#6554,#3953,.T.);
#8416=EDGE_CURVE('',#6556,#6541,#403,.T.);
#8417=EDGE_CURVE('',#6556,#6534,#404,.T.);
#8418=EDGE_CURVE('',#6540,#6516,#3954,.T.);
#8419=EDGE_CURVE('',#6516,#6556,#405,.T.);
#8420=EDGE_CURVE('',#6517,#6539,#3955,.T.);
#8421=EDGE_CURVE('',#6538,#6518,#3956,.T.);
#8422=EDGE_CURVE('',#6555,#6519,#406,.T.);
#8423=EDGE_CURVE('',#6519,#6537,#3957,.T.);
#8424=EDGE_CURVE('',#6554,#6549,#3958,.T.);
#8425=EDGE_CURVE('',#6450,#6557,#3959,.T.);
#8426=EDGE_CURVE('',#6557,#6468,#1091,.T.);
#8427=EDGE_CURVE('',#6448,#6558,#3960,.T.);
#8428=EDGE_CURVE('',#6558,#6557,#3961,.T.);
#8429=EDGE_CURVE('',#6446,#6559,#3962,.T.);
#8430=EDGE_CURVE('',#6559,#6558,#1092,.T.);
#8431=EDGE_CURVE('',#6465,#6559,#3963,.T.);
#8432=EDGE_CURVE('',#6560,#6560,#1093,.T.);
#8433=EDGE_CURVE('',#6560,#6561,#3964,.T.);
#8434=EDGE_CURVE('',#6561,#6561,#1094,.T.);
#8435=EDGE_CURVE('',#6562,#6562,#1095,.T.);
#8436=EDGE_CURVE('',#6562,#6560,#3965,.T.);
#8437=EDGE_CURVE('',#6563,#6564,#3966,.T.);
#8438=EDGE_CURVE('',#6565,#6563,#3967,.T.);
#8439=EDGE_CURVE('',#6566,#6565,#3968,.T.);
#8440=EDGE_CURVE('',#6567,#6566,#3969,.T.);
#8441=EDGE_CURVE('',#6568,#6567,#3970,.T.);
#8442=EDGE_CURVE('',#6569,#6568,#3971,.T.);
#8443=EDGE_CURVE('',#6570,#6569,#3972,.T.);
#8444=EDGE_CURVE('',#6571,#6570,#3973,.T.);
#8445=EDGE_CURVE('',#6572,#6571,#3974,.T.);
#8446=EDGE_CURVE('',#6564,#6572,#3975,.T.);
#8447=EDGE_CURVE('',#6573,#6573,#1096,.T.);
#8448=EDGE_CURVE('',#6573,#6562,#3976,.T.);
#8449=EDGE_CURVE('',#6574,#6575,#3977,.T.);
#8450=EDGE_CURVE('',#6575,#6576,#3978,.T.);
#8451=EDGE_CURVE('',#6577,#6576,#3979,.T.);
#8452=EDGE_CURVE('',#6577,#6578,#3980,.T.);
#8453=EDGE_CURVE('',#6578,#6579,#3981,.T.);
#8454=EDGE_CURVE('',#6580,#6579,#3982,.T.);
#8455=EDGE_CURVE('',#6580,#6581,#3983,.T.);
#8456=EDGE_CURVE('',#6581,#6582,#3984,.T.);
#8457=EDGE_CURVE('',#6583,#6582,#3985,.T.);
#8458=EDGE_CURVE('',#6583,#6584,#3986,.T.);
#8459=EDGE_CURVE('',#6584,#6585,#3987,.T.);
#8460=EDGE_CURVE('',#6586,#6585,#3988,.T.);
#8461=EDGE_CURVE('',#6586,#6587,#3989,.T.);
#8462=EDGE_CURVE('',#6587,#6588,#3990,.T.);
#8463=EDGE_CURVE('',#6589,#6588,#3991,.T.);
#8464=EDGE_CURVE('',#6589,#6590,#3992,.T.);
#8465=EDGE_CURVE('',#6590,#6591,#3993,.T.);
#8466=EDGE_CURVE('',#6592,#6591,#3994,.T.);
#8467=EDGE_CURVE('',#6592,#6593,#3995,.T.);
#8468=EDGE_CURVE('',#6593,#6594,#3996,.T.);
#8469=EDGE_CURVE('',#6595,#6594,#3997,.T.);
#8470=EDGE_CURVE('',#6595,#6596,#3998,.T.);
#8471=EDGE_CURVE('',#6596,#6597,#3999,.T.);
#8472=EDGE_CURVE('',#6598,#6597,#4000,.T.);
#8473=EDGE_CURVE('',#6598,#6599,#4001,.T.);
#8474=EDGE_CURVE('',#6599,#6600,#4002,.T.);
#8475=EDGE_CURVE('',#6601,#6600,#4003,.T.);
#8476=EDGE_CURVE('',#6601,#6602,#4004,.T.);
#8477=EDGE_CURVE('',#6602,#6603,#4005,.T.);
#8478=EDGE_CURVE('',#6604,#6603,#4006,.T.);
#8479=EDGE_CURVE('',#6604,#6605,#4007,.T.);
#8480=EDGE_CURVE('',#6605,#6606,#4008,.T.);
#8481=EDGE_CURVE('',#6607,#6606,#4009,.T.);
#8482=EDGE_CURVE('',#6607,#6608,#4010,.T.);
#8483=EDGE_CURVE('',#6608,#6609,#4011,.T.);
#8484=EDGE_CURVE('',#6610,#6609,#4012,.T.);
#8485=EDGE_CURVE('',#6610,#6611,#4013,.T.);
#8486=EDGE_CURVE('',#6611,#6612,#4014,.T.);
#8487=EDGE_CURVE('',#6613,#6612,#4015,.T.);
#8488=EDGE_CURVE('',#6613,#6614,#4016,.T.);
#8489=EDGE_CURVE('',#6614,#6615,#4017,.T.);
#8490=EDGE_CURVE('',#6616,#6615,#4018,.T.);
#8491=EDGE_CURVE('',#6616,#6617,#4019,.T.);
#8492=EDGE_CURVE('',#6617,#6618,#4020,.T.);
#8493=EDGE_CURVE('',#6619,#6618,#4021,.T.);
#8494=EDGE_CURVE('',#6619,#6620,#4022,.T.);
#8495=EDGE_CURVE('',#6620,#6621,#4023,.T.);
#8496=EDGE_CURVE('',#6622,#6621,#4024,.T.);
#8497=EDGE_CURVE('',#6622,#6623,#4025,.T.);
#8498=EDGE_CURVE('',#6623,#6624,#4026,.T.);
#8499=EDGE_CURVE('',#6625,#6624,#4027,.T.);
#8500=EDGE_CURVE('',#6625,#6626,#4028,.T.);
#8501=EDGE_CURVE('',#6626,#6627,#4029,.T.);
#8502=EDGE_CURVE('',#6628,#6627,#4030,.T.);
#8503=EDGE_CURVE('',#6628,#6629,#4031,.T.);
#8504=EDGE_CURVE('',#6629,#6630,#4032,.T.);
#8505=EDGE_CURVE('',#6631,#6630,#4033,.T.);
#8506=EDGE_CURVE('',#6631,#6632,#4034,.T.);
#8507=EDGE_CURVE('',#6632,#6633,#4035,.T.);
#8508=EDGE_CURVE('',#6574,#6633,#4036,.T.);
#8509=EDGE_CURVE('',#6633,#6634,#4037,.F.);
#8510=EDGE_CURVE('',#6634,#6635,#4038,.T.);
#8511=EDGE_CURVE('',#6635,#6574,#4039,.F.);
#8512=EDGE_CURVE('',#6636,#6634,#4040,.T.);
#8513=EDGE_CURVE('',#6636,#6637,#4041,.T.);
#8514=EDGE_CURVE('',#6637,#6635,#4042,.T.);
#8515=EDGE_CURVE('',#6579,#6638,#4043,.F.);
#8516=EDGE_CURVE('',#6638,#6639,#4044,.T.);
#8517=EDGE_CURVE('',#6639,#6580,#4045,.F.);
#8518=EDGE_CURVE('',#6640,#6638,#4046,.T.);
#8519=EDGE_CURVE('',#6640,#6641,#4047,.T.);
#8520=EDGE_CURVE('',#6641,#6639,#4048,.T.);
#8521=EDGE_CURVE('',#6585,#6642,#4049,.F.);
#8522=EDGE_CURVE('',#6642,#6643,#4050,.T.);
#8523=EDGE_CURVE('',#6643,#6586,#4051,.F.);
#8524=EDGE_CURVE('',#6644,#6642,#4052,.T.);
#8525=EDGE_CURVE('',#6644,#6645,#4053,.T.);
#8526=EDGE_CURVE('',#6645,#6643,#4054,.T.);
#8527=EDGE_CURVE('',#6646,#6647,#4055,.T.);
#8528=EDGE_CURVE('',#6564,#6646,#4056,.T.);
#8529=EDGE_CURVE('',#6647,#6564,#4057,.T.);
#8530=EDGE_CURVE('',#6648,#6563,#4058,.T.);
#8531=EDGE_CURVE('',#6646,#6649,#4059,.T.);
#8532=EDGE_CURVE('',#6649,#6648,#4060,.T.);
#8533=EDGE_CURVE('',#6650,#6651,#4061,.T.);
#8534=EDGE_CURVE('',#6572,#6650,#4062,.T.);
#8535=EDGE_CURVE('',#6651,#6572,#4063,.T.);
#8536=EDGE_CURVE('',#6650,#6647,#4064,.T.);
#8537=EDGE_CURVE('',#6652,#6653,#4065,.T.);
#8538=EDGE_CURVE('',#6571,#6652,#4066,.T.);
#8539=EDGE_CURVE('',#6653,#6571,#4067,.T.);
#8540=EDGE_CURVE('',#6652,#6651,#4068,.T.);
#8541=EDGE_CURVE('',#6654,#6655,#4069,.T.);
#8542=EDGE_CURVE('',#6655,#6653,#4070,.T.);
#8543=EDGE_CURVE('',#6570,#6654,#4071,.T.);
#8544=EDGE_CURVE('',#6588,#6652,#4072,.T.);
#8545=EDGE_CURVE('',#6653,#6589,#4073,.T.);
#8546=EDGE_CURVE('',#6582,#6650,#4074,.T.);
#8547=EDGE_CURVE('',#6651,#6583,#4075,.T.);
#8548=EDGE_CURVE('',#6576,#6646,#4076,.T.);
#8549=EDGE_CURVE('',#6647,#6577,#4077,.T.);
#8550=EDGE_CURVE('',#6581,#6656,#4078,.T.);
#8551=EDGE_CURVE('',#6656,#6657,#4079,.T.);
#8552=EDGE_CURVE('',#6657,#6578,#4080,.T.);
#8553=EDGE_CURVE('',#6587,#6658,#4081,.T.);
#8554=EDGE_CURVE('',#6658,#6659,#4082,.T.);
#8555=EDGE_CURVE('',#6659,#6584,#4083,.T.);
#8556=EDGE_CURVE('',#6594,#6655,#4084,.T.);
#8557=EDGE_CURVE('',#6593,#6660,#4085,.T.);
#8558=EDGE_CURVE('',#6660,#6661,#4086,.T.);
#8559=EDGE_CURVE('',#6661,#6590,#4087,.T.);
#8560=EDGE_CURVE('',#6662,#6654,#4088,.T.);
#8561=EDGE_CURVE('',#6662,#6595,#4089,.T.);
#8562=EDGE_CURVE('',#6569,#6663,#4090,.T.);
#8563=EDGE_CURVE('',#6663,#6662,#4091,.T.);
#8564=EDGE_CURVE('',#6591,#6664,#4092,.F.);
#8565=EDGE_CURVE('',#6664,#6665,#4093,.T.);
#8566=EDGE_CURVE('',#6665,#6592,#4094,.F.);
#8567=EDGE_CURVE('',#6666,#6664,#4095,.T.);
#8568=EDGE_CURVE('',#6666,#6667,#4096,.T.);
#8569=EDGE_CURVE('',#6667,#6665,#4097,.T.);
#8570=EDGE_CURVE('',#6597,#6668,#4098,.F.);
#8571=EDGE_CURVE('',#6668,#6669,#4099,.T.);
#8572=EDGE_CURVE('',#6669,#6598,#4100,.F.);
#8573=EDGE_CURVE('',#6670,#6668,#4101,.T.);
#8574=EDGE_CURVE('',#6670,#6671,#4102,.T.);
#8575=EDGE_CURVE('',#6671,#6669,#4103,.T.);
#8576=EDGE_CURVE('',#6603,#6672,#4104,.F.);
#8577=EDGE_CURVE('',#6672,#6673,#4105,.T.);
#8578=EDGE_CURVE('',#6673,#6604,#4106,.F.);
#8579=EDGE_CURVE('',#6674,#6672,#4107,.T.);
#8580=EDGE_CURVE('',#6674,#6675,#4108,.T.);
#8581=EDGE_CURVE('',#6675,#6673,#4109,.T.);
#8582=EDGE_CURVE('',#6609,#6676,#4110,.F.);
#8583=EDGE_CURVE('',#6676,#6677,#4111,.T.);
#8584=EDGE_CURVE('',#6677,#6610,#4112,.F.);
#8585=EDGE_CURVE('',#6678,#6676,#4113,.T.);
#8586=EDGE_CURVE('',#6678,#6679,#4114,.T.);
#8587=EDGE_CURVE('',#6679,#6677,#4115,.T.);
#8588=EDGE_CURVE('',#6615,#6680,#4116,.F.);
#8589=EDGE_CURVE('',#6680,#6681,#4117,.T.);
#8590=EDGE_CURVE('',#6681,#6616,#4118,.F.);
#8591=EDGE_CURVE('',#6682,#6680,#4119,.T.);
#8592=EDGE_CURVE('',#6682,#6683,#4120,.T.);
#8593=EDGE_CURVE('',#6683,#6681,#4121,.T.);
#8594=EDGE_CURVE('',#6621,#6684,#4122,.F.);
#8595=EDGE_CURVE('',#6684,#6685,#4123,.T.);
#8596=EDGE_CURVE('',#6685,#6622,#4124,.F.);
#8597=EDGE_CURVE('',#6686,#6684,#4125,.T.);
#8598=EDGE_CURVE('',#6686,#6687,#4126,.T.);
#8599=EDGE_CURVE('',#6687,#6685,#4127,.T.);
#8600=EDGE_CURVE('',#6663,#6688,#4128,.T.);
#8601=EDGE_CURVE('',#6688,#6569,#4129,.T.);
#8602=EDGE_CURVE('',#6689,#6690,#4130,.T.);
#8603=EDGE_CURVE('',#6568,#6689,#4131,.T.);
#8604=EDGE_CURVE('',#6690,#6568,#4132,.T.);
#8605=EDGE_CURVE('',#6689,#6688,#4133,.T.);
#8606=EDGE_CURVE('',#6691,#6692,#4134,.T.);
#8607=EDGE_CURVE('',#6567,#6691,#4135,.T.);
#8608=EDGE_CURVE('',#6692,#6567,#4136,.T.);
#8609=EDGE_CURVE('',#6691,#6690,#4137,.T.);
#8610=EDGE_CURVE('',#6693,#6694,#4138,.T.);
#8611=EDGE_CURVE('',#6566,#6693,#4139,.T.);
#8612=EDGE_CURVE('',#6694,#6566,#4140,.T.);
#8613=EDGE_CURVE('',#6693,#6692,#4141,.T.);
#8614=EDGE_CURVE('',#6565,#6695,#4142,.T.);
#8615=EDGE_CURVE('',#6696,#6565,#4143,.T.);
#8616=EDGE_CURVE('',#6695,#6696,#4144,.T.);
#8617=EDGE_CURVE('',#6648,#6697,#4145,.T.);
#8618=EDGE_CURVE('',#6697,#6696,#4146,.T.);
#8619=EDGE_CURVE('',#6624,#6695,#4147,.T.);
#8620=EDGE_CURVE('',#6696,#6625,#4148,.T.);
#8621=EDGE_CURVE('',#6695,#6694,#4149,.T.);
#8622=EDGE_CURVE('',#6649,#6631,#4150,.T.);
#8623=EDGE_CURVE('',#6630,#6697,#4151,.T.);
#8624=EDGE_CURVE('',#6618,#6693,#4152,.T.);
#8625=EDGE_CURVE('',#6694,#6619,#4153,.T.);
#8626=EDGE_CURVE('',#6612,#6691,#4154,.T.);
#8627=EDGE_CURVE('',#6692,#6613,#4155,.T.);
#8628=EDGE_CURVE('',#6606,#6689,#4156,.T.);
#8629=EDGE_CURVE('',#6690,#6607,#4157,.T.);
#8630=EDGE_CURVE('',#6600,#6663,#4158,.T.);
#8631=EDGE_CURVE('',#6688,#6601,#4159,.T.);
#8632=EDGE_CURVE('',#6599,#6698,#4160,.T.);
#8633=EDGE_CURVE('',#6698,#6699,#4161,.T.);
#8634=EDGE_CURVE('',#6699,#6596,#4162,.T.);
#8635=EDGE_CURVE('',#6605,#6700,#4163,.T.);
#8636=EDGE_CURVE('',#6700,#6701,#4164,.T.);
#8637=EDGE_CURVE('',#6701,#6602,#4165,.T.);
#8638=EDGE_CURVE('',#6611,#6702,#4166,.T.);
#8639=EDGE_CURVE('',#6702,#6703,#4167,.T.);
#8640=EDGE_CURVE('',#6703,#6608,#4168,.T.);
#8641=EDGE_CURVE('',#6617,#6704,#4169,.T.);
#8642=EDGE_CURVE('',#6704,#6705,#4170,.T.);
#8643=EDGE_CURVE('',#6705,#6614,#4171,.T.);
#8644=EDGE_CURVE('',#6623,#6706,#4172,.T.);
#8645=EDGE_CURVE('',#6706,#6707,#4173,.T.);
#8646=EDGE_CURVE('',#6707,#6620,#4174,.T.);
#8647=EDGE_CURVE('',#6627,#6708,#4175,.F.);
#8648=EDGE_CURVE('',#6708,#6709,#4176,.T.);
#8649=EDGE_CURVE('',#6709,#6628,#4177,.F.);
#8650=EDGE_CURVE('',#6710,#6708,#4178,.T.);
#8651=EDGE_CURVE('',#6710,#6711,#4179,.T.);
#8652=EDGE_CURVE('',#6711,#6709,#4180,.T.);
#8653=EDGE_CURVE('',#6712,#6713,#4181,.T.);
#8654=EDGE_CURVE('',#6711,#6712,#4182,.T.);
#8655=EDGE_CURVE('',#6713,#6710,#4183,.T.);
#8656=EDGE_CURVE('',#6713,#6626,#4184,.T.);
#8657=EDGE_CURVE('',#6629,#6712,#4185,.T.);
#8658=EDGE_CURVE('',#6687,#6706,#4186,.T.);
#8659=EDGE_CURVE('',#6707,#6686,#4187,.T.);
#8660=EDGE_CURVE('',#6683,#6704,#4188,.T.);
#8661=EDGE_CURVE('',#6705,#6682,#4189,.T.);
#8662=EDGE_CURVE('',#6679,#6702,#4190,.T.);
#8663=EDGE_CURVE('',#6703,#6678,#4191,.T.);
#8664=EDGE_CURVE('',#6675,#6700,#4192,.T.);
#8665=EDGE_CURVE('',#6701,#6674,#4193,.T.);
#8666=EDGE_CURVE('',#6671,#6698,#4194,.T.);
#8667=EDGE_CURVE('',#6699,#6670,#4195,.T.);
#8668=EDGE_CURVE('',#6667,#6660,#4196,.T.);
#8669=EDGE_CURVE('',#6661,#6666,#4197,.T.);
#8670=EDGE_CURVE('',#6645,#6658,#4198,.T.);
#8671=EDGE_CURVE('',#6659,#6644,#4199,.T.);
#8672=EDGE_CURVE('',#6641,#6656,#4200,.T.);
#8673=EDGE_CURVE('',#6657,#6640,#4201,.T.);
#8674=EDGE_CURVE('',#6714,#6632,#4202,.T.);
#8675=EDGE_CURVE('',#6714,#6636,#4203,.T.);
#8676=EDGE_CURVE('',#6575,#6715,#4204,.T.);
#8677=EDGE_CURVE('',#6637,#6715,#4205,.T.);
#8678=EDGE_CURVE('',#6715,#6714,#4206,.T.);
#8679=ORIENTED_EDGE('',*,*,#6716,.T.);
#8680=ORIENTED_EDGE('',*,*,#6717,.T.);
#8681=ORIENTED_EDGE('',*,*,#6718,.T.);
#8682=ORIENTED_EDGE('',*,*,#6719,.T.);
#8683=ORIENTED_EDGE('',*,*,#6720,.T.);
#8684=ORIENTED_EDGE('',*,*,#6721,.T.);
#8685=ORIENTED_EDGE('',*,*,#6716,.F.);
#8686=ORIENTED_EDGE('',*,*,#6722,.T.);
#8687=ORIENTED_EDGE('',*,*,#6723,.T.);
#8688=ORIENTED_EDGE('',*,*,#6724,.T.);
#8689=ORIENTED_EDGE('',*,*,#6720,.F.);
#8690=ORIENTED_EDGE('',*,*,#6725,.T.);
#8691=ORIENTED_EDGE('',*,*,#6726,.T.);
#8692=ORIENTED_EDGE('',*,*,#6727,.T.);
#8693=ORIENTED_EDGE('',*,*,#6723,.F.);
#8694=ORIENTED_EDGE('',*,*,#6728,.T.);
#8695=ORIENTED_EDGE('',*,*,#6729,.T.);
#8696=ORIENTED_EDGE('',*,*,#6730,.T.);
#8697=ORIENTED_EDGE('',*,*,#6726,.F.);
#8698=ORIENTED_EDGE('',*,*,#6731,.T.);
#8699=ORIENTED_EDGE('',*,*,#6732,.T.);
#8700=ORIENTED_EDGE('',*,*,#6733,.T.);
#8701=ORIENTED_EDGE('',*,*,#6729,.F.);
#8702=ORIENTED_EDGE('',*,*,#6734,.T.);
#8703=ORIENTED_EDGE('',*,*,#6735,.T.);
#8704=ORIENTED_EDGE('',*,*,#6736,.T.);
#8705=ORIENTED_EDGE('',*,*,#6732,.F.);
#8706=ORIENTED_EDGE('',*,*,#6737,.T.);
#8707=ORIENTED_EDGE('',*,*,#6718,.F.);
#8708=ORIENTED_EDGE('',*,*,#6738,.T.);
#8709=ORIENTED_EDGE('',*,*,#6735,.F.);
#8710=ORIENTED_EDGE('',*,*,#6739,.T.);
#8711=ORIENTED_EDGE('',*,*,#6728,.F.);
#8712=ORIENTED_EDGE('',*,*,#6740,.F.);
#8713=ORIENTED_EDGE('',*,*,#6741,.F.);
#8714=ORIENTED_EDGE('',*,*,#6742,.T.);
#8715=ORIENTED_EDGE('',*,*,#6725,.F.);
#8716=ORIENTED_EDGE('',*,*,#6743,.F.);
#8717=ORIENTED_EDGE('',*,*,#6744,.F.);
#8718=ORIENTED_EDGE('',*,*,#6740,.T.);
#8719=ORIENTED_EDGE('',*,*,#6745,.T.);
#8720=ORIENTED_EDGE('',*,*,#6722,.F.);
#8721=ORIENTED_EDGE('',*,*,#6746,.F.);
#8722=ORIENTED_EDGE('',*,*,#6747,.F.);
#8723=ORIENTED_EDGE('',*,*,#6743,.T.);
#8724=ORIENTED_EDGE('',*,*,#6719,.F.);
#8725=ORIENTED_EDGE('',*,*,#6748,.F.);
#8726=ORIENTED_EDGE('',*,*,#6749,.F.);
#8727=ORIENTED_EDGE('',*,*,#6746,.T.);
#8728=ORIENTED_EDGE('',*,*,#6750,.F.);
#8729=ORIENTED_EDGE('',*,*,#6751,.F.);
#8730=ORIENTED_EDGE('',*,*,#6752,.F.);
#8731=ORIENTED_EDGE('',*,*,#6753,.F.);
#8732=ORIENTED_EDGE('',*,*,#6754,.F.);
#8733=ORIENTED_EDGE('',*,*,#6755,.F.);
#8734=ORIENTED_EDGE('',*,*,#6756,.F.);
#8735=ORIENTED_EDGE('',*,*,#6757,.F.);
#8736=ORIENTED_EDGE('',*,*,#6717,.F.);
#8737=ORIENTED_EDGE('',*,*,#6721,.F.);
#8738=ORIENTED_EDGE('',*,*,#6724,.F.);
#8739=ORIENTED_EDGE('',*,*,#6727,.F.);
#8740=ORIENTED_EDGE('',*,*,#6730,.F.);
#8741=ORIENTED_EDGE('',*,*,#6733,.F.);
#8742=ORIENTED_EDGE('',*,*,#6736,.F.);
#8743=ORIENTED_EDGE('',*,*,#6738,.F.);
#8744=ORIENTED_EDGE('',*,*,#6758,.T.);
#8745=ORIENTED_EDGE('',*,*,#6750,.T.);
#8746=ORIENTED_EDGE('',*,*,#6759,.T.);
#8747=ORIENTED_EDGE('',*,*,#6760,.T.);
#8748=ORIENTED_EDGE('',*,*,#6761,.T.);
#8749=ORIENTED_EDGE('',*,*,#6751,.T.);
#8750=ORIENTED_EDGE('',*,*,#6758,.F.);
#8751=ORIENTED_EDGE('',*,*,#6762,.T.);
#8752=ORIENTED_EDGE('',*,*,#6763,.T.);
#8753=ORIENTED_EDGE('',*,*,#6752,.T.);
#8754=ORIENTED_EDGE('',*,*,#6761,.F.);
#8755=ORIENTED_EDGE('',*,*,#6764,.T.);
#8756=ORIENTED_EDGE('',*,*,#6765,.T.);
#8757=ORIENTED_EDGE('',*,*,#6753,.T.);
#8758=ORIENTED_EDGE('',*,*,#6763,.F.);
#8759=ORIENTED_EDGE('',*,*,#6766,.T.);
#8760=ORIENTED_EDGE('',*,*,#6767,.T.);
#8761=ORIENTED_EDGE('',*,*,#6754,.T.);
#8762=ORIENTED_EDGE('',*,*,#6765,.F.);
#8763=ORIENTED_EDGE('',*,*,#6768,.T.);
#8764=ORIENTED_EDGE('',*,*,#6769,.T.);
#8765=ORIENTED_EDGE('',*,*,#6755,.T.);
#8766=ORIENTED_EDGE('',*,*,#6767,.F.);
#8767=ORIENTED_EDGE('',*,*,#6770,.T.);
#8768=ORIENTED_EDGE('',*,*,#6771,.T.);
#8769=ORIENTED_EDGE('',*,*,#6756,.T.);
#8770=ORIENTED_EDGE('',*,*,#6769,.F.);
#8771=ORIENTED_EDGE('',*,*,#6772,.T.);
#8772=ORIENTED_EDGE('',*,*,#6759,.F.);
#8773=ORIENTED_EDGE('',*,*,#6757,.T.);
#8774=ORIENTED_EDGE('',*,*,#6771,.F.);
#8775=ORIENTED_EDGE('',*,*,#6773,.T.);
#8776=ORIENTED_EDGE('',*,*,#6766,.F.);
#8777=ORIENTED_EDGE('',*,*,#6774,.F.);
#8778=ORIENTED_EDGE('',*,*,#6775,.F.);
#8779=ORIENTED_EDGE('',*,*,#6776,.T.);
#8780=ORIENTED_EDGE('',*,*,#6764,.F.);
#8781=ORIENTED_EDGE('',*,*,#6777,.F.);
#8782=ORIENTED_EDGE('',*,*,#6778,.F.);
#8783=ORIENTED_EDGE('',*,*,#6774,.T.);
#8784=ORIENTED_EDGE('',*,*,#6762,.F.);
#8785=ORIENTED_EDGE('',*,*,#6779,.F.);
#8786=ORIENTED_EDGE('',*,*,#6780,.F.);
#8787=ORIENTED_EDGE('',*,*,#6777,.T.);
#8788=ORIENTED_EDGE('',*,*,#6760,.F.);
#8789=ORIENTED_EDGE('',*,*,#6781,.F.);
#8790=ORIENTED_EDGE('',*,*,#6782,.F.);
#8791=ORIENTED_EDGE('',*,*,#6779,.T.);
#8792=ORIENTED_EDGE('',*,*,#6783,.T.);
#8793=ORIENTED_EDGE('',*,*,#6778,.T.);
#8794=ORIENTED_EDGE('',*,*,#6784,.T.);
#8795=ORIENTED_EDGE('',*,*,#6785,.T.);
#8796=ORIENTED_EDGE('',*,*,#6786,.T.);
#8797=ORIENTED_EDGE('',*,*,#6775,.T.);
#8798=ORIENTED_EDGE('',*,*,#6783,.F.);
#8799=ORIENTED_EDGE('',*,*,#6787,.T.);
#8800=ORIENTED_EDGE('',*,*,#6788,.T.);
#8801=ORIENTED_EDGE('',*,*,#6789,.T.);
#8802=ORIENTED_EDGE('',*,*,#6786,.F.);
#8803=ORIENTED_EDGE('',*,*,#6790,.T.);
#8804=ORIENTED_EDGE('',*,*,#6791,.T.);
#8805=ORIENTED_EDGE('',*,*,#6792,.T.);
#8806=ORIENTED_EDGE('',*,*,#6788,.F.);
#8807=ORIENTED_EDGE('',*,*,#6793,.T.);
#8808=ORIENTED_EDGE('',*,*,#6794,.T.);
#8809=ORIENTED_EDGE('',*,*,#6795,.T.);
#8810=ORIENTED_EDGE('',*,*,#6791,.F.);
#8811=ORIENTED_EDGE('',*,*,#6796,.T.);
#8812=ORIENTED_EDGE('',*,*,#6797,.T.);
#8813=ORIENTED_EDGE('',*,*,#6798,.T.);
#8814=ORIENTED_EDGE('',*,*,#6794,.F.);
#8815=ORIENTED_EDGE('',*,*,#6799,.T.);
#8816=ORIENTED_EDGE('',*,*,#6800,.T.);
#8817=ORIENTED_EDGE('',*,*,#6782,.T.);
#8818=ORIENTED_EDGE('',*,*,#6797,.F.);
#8819=ORIENTED_EDGE('',*,*,#6801,.T.);
#8820=ORIENTED_EDGE('',*,*,#6784,.F.);
#8821=ORIENTED_EDGE('',*,*,#6780,.T.);
#8822=ORIENTED_EDGE('',*,*,#6800,.F.);
#8823=ORIENTED_EDGE('',*,*,#6802,.T.);
#8824=ORIENTED_EDGE('',*,*,#6773,.F.);
#8825=ORIENTED_EDGE('',*,*,#6803,.F.);
#8826=ORIENTED_EDGE('',*,*,#6798,.F.);
#8827=ORIENTED_EDGE('',*,*,#6781,.T.);
#8828=ORIENTED_EDGE('',*,*,#6785,.F.);
#8829=ORIENTED_EDGE('',*,*,#6802,.F.);
#8830=ORIENTED_EDGE('',*,*,#6801,.F.);
#8831=ORIENTED_EDGE('',*,*,#6799,.F.);
#8832=ORIENTED_EDGE('',*,*,#6796,.F.);
#8833=ORIENTED_EDGE('',*,*,#6793,.F.);
#8834=ORIENTED_EDGE('',*,*,#6790,.F.);
#8835=ORIENTED_EDGE('',*,*,#6787,.F.);
#8836=ORIENTED_EDGE('',*,*,#6804,.F.);
#8837=ORIENTED_EDGE('',*,*,#6805,.F.);
#8838=ORIENTED_EDGE('',*,*,#6806,.F.);
#8839=ORIENTED_EDGE('',*,*,#6807,.F.);
#8840=ORIENTED_EDGE('',*,*,#6808,.F.);
#8841=ORIENTED_EDGE('',*,*,#6809,.F.);
#8842=ORIENTED_EDGE('',*,*,#6810,.F.);
#8843=ORIENTED_EDGE('',*,*,#6811,.F.);
#8844=ORIENTED_EDGE('',*,*,#6812,.T.);
#8845=ORIENTED_EDGE('',*,*,#6744,.T.);
#8846=ORIENTED_EDGE('',*,*,#6813,.T.);
#8847=ORIENTED_EDGE('',*,*,#6804,.T.);
#8848=ORIENTED_EDGE('',*,*,#6814,.T.);
#8849=ORIENTED_EDGE('',*,*,#6741,.T.);
#8850=ORIENTED_EDGE('',*,*,#6812,.F.);
#8851=ORIENTED_EDGE('',*,*,#6811,.T.);
#8852=ORIENTED_EDGE('',*,*,#6815,.T.);
#8853=ORIENTED_EDGE('',*,*,#6816,.T.);
#8854=ORIENTED_EDGE('',*,*,#6814,.F.);
#8855=ORIENTED_EDGE('',*,*,#6810,.T.);
#8856=ORIENTED_EDGE('',*,*,#6817,.T.);
#8857=ORIENTED_EDGE('',*,*,#6818,.T.);
#8858=ORIENTED_EDGE('',*,*,#6815,.F.);
#8859=ORIENTED_EDGE('',*,*,#6809,.T.);
#8860=ORIENTED_EDGE('',*,*,#6819,.T.);
#8861=ORIENTED_EDGE('',*,*,#6820,.T.);
#8862=ORIENTED_EDGE('',*,*,#6817,.F.);
#8863=ORIENTED_EDGE('',*,*,#6808,.T.);
#8864=ORIENTED_EDGE('',*,*,#6821,.T.);
#8865=ORIENTED_EDGE('',*,*,#6822,.T.);
#8866=ORIENTED_EDGE('',*,*,#6819,.F.);
#8867=ORIENTED_EDGE('',*,*,#6807,.T.);
#8868=ORIENTED_EDGE('',*,*,#6823,.T.);
#8869=ORIENTED_EDGE('',*,*,#6749,.T.);
#8870=ORIENTED_EDGE('',*,*,#6821,.F.);
#8871=ORIENTED_EDGE('',*,*,#6806,.T.);
#8872=ORIENTED_EDGE('',*,*,#6813,.F.);
#8873=ORIENTED_EDGE('',*,*,#6747,.T.);
#8874=ORIENTED_EDGE('',*,*,#6823,.F.);
#8875=ORIENTED_EDGE('',*,*,#6805,.T.);
#8876=ORIENTED_EDGE('',*,*,#6739,.F.);
#8877=ORIENTED_EDGE('',*,*,#6824,.F.);
#8878=ORIENTED_EDGE('',*,*,#6822,.F.);
#8879=ORIENTED_EDGE('',*,*,#6748,.T.);
#8880=ORIENTED_EDGE('',*,*,#6825,.F.);
#8881=ORIENTED_EDGE('',*,*,#6826,.T.);
#8882=ORIENTED_EDGE('',*,*,#6745,.F.);
#8883=ORIENTED_EDGE('',*,*,#6826,.F.);
#8884=ORIENTED_EDGE('',*,*,#6737,.F.);
#8885=ORIENTED_EDGE('',*,*,#6827,.F.);
#8886=ORIENTED_EDGE('',*,*,#6820,.F.);
#8887=ORIENTED_EDGE('',*,*,#6824,.T.);
#8888=ORIENTED_EDGE('',*,*,#6734,.F.);
#8889=ORIENTED_EDGE('',*,*,#6828,.F.);
#8890=ORIENTED_EDGE('',*,*,#6818,.F.);
#8891=ORIENTED_EDGE('',*,*,#6827,.T.);
#8892=ORIENTED_EDGE('',*,*,#6731,.F.);
#8893=ORIENTED_EDGE('',*,*,#6742,.F.);
#8894=ORIENTED_EDGE('',*,*,#6816,.F.);
#8895=ORIENTED_EDGE('',*,*,#6828,.T.);
#8896=ORIENTED_EDGE('',*,*,#6772,.F.);
#8897=ORIENTED_EDGE('',*,*,#6829,.F.);
#8898=ORIENTED_EDGE('',*,*,#6795,.F.);
#8899=ORIENTED_EDGE('',*,*,#6803,.T.);
#8900=ORIENTED_EDGE('',*,*,#6770,.F.);
#8901=ORIENTED_EDGE('',*,*,#6830,.F.);
#8902=ORIENTED_EDGE('',*,*,#6792,.F.);
#8903=ORIENTED_EDGE('',*,*,#6829,.T.);
#8904=ORIENTED_EDGE('',*,*,#6768,.F.);
#8905=ORIENTED_EDGE('',*,*,#6776,.F.);
#8906=ORIENTED_EDGE('',*,*,#6789,.F.);
#8907=ORIENTED_EDGE('',*,*,#6830,.T.);
#8908=ORIENTED_EDGE('',*,*,#6825,.T.);
#8909=ORIENTED_EDGE('',*,*,#6831,.T.);
#8910=ORIENTED_EDGE('',*,*,#6832,.F.);
#8911=ORIENTED_EDGE('',*,*,#6833,.T.);
#8912=ORIENTED_EDGE('',*,*,#6834,.T.);
#8913=ORIENTED_EDGE('',*,*,#6835,.T.);
#8914=ORIENTED_EDGE('',*,*,#6836,.F.);
#8915=ORIENTED_EDGE('',*,*,#6837,.T.);
#8916=ORIENTED_EDGE('',*,*,#6838,.T.);
#8917=ORIENTED_EDGE('',*,*,#6836,.T.);
#8918=ORIENTED_EDGE('',*,*,#6839,.T.);
#8919=ORIENTED_EDGE('',*,*,#6840,.T.);
#8920=ORIENTED_EDGE('',*,*,#6841,.T.);
#8921=ORIENTED_EDGE('',*,*,#6842,.T.);
#8922=ORIENTED_EDGE('',*,*,#6843,.T.);
#8923=ORIENTED_EDGE('',*,*,#6844,.T.);
#8924=ORIENTED_EDGE('',*,*,#6845,.T.);
#8925=ORIENTED_EDGE('',*,*,#6842,.F.);
#8926=ORIENTED_EDGE('',*,*,#6846,.T.);
#8927=ORIENTED_EDGE('',*,*,#6840,.F.);
#8928=ORIENTED_EDGE('',*,*,#6847,.T.);
#8929=ORIENTED_EDGE('',*,*,#6832,.T.);
#8930=ORIENTED_EDGE('',*,*,#6848,.T.);
#8931=ORIENTED_EDGE('',*,*,#6849,.T.);
#8932=ORIENTED_EDGE('',*,*,#6850,.T.);
#8933=ORIENTED_EDGE('',*,*,#6849,.F.);
#8934=ORIENTED_EDGE('',*,*,#6851,.T.);
#8935=ORIENTED_EDGE('',*,*,#6844,.F.);
#8936=ORIENTED_EDGE('',*,*,#6852,.T.);
#8937=ORIENTED_EDGE('',*,*,#6848,.F.);
#8938=ORIENTED_EDGE('',*,*,#6831,.F.);
#8939=ORIENTED_EDGE('',*,*,#6853,.T.);
#8940=ORIENTED_EDGE('',*,*,#6854,.F.);
#8941=ORIENTED_EDGE('',*,*,#6855,.F.);
#8942=ORIENTED_EDGE('',*,*,#6856,.T.);
#8943=ORIENTED_EDGE('',*,*,#6834,.F.);
#8944=ORIENTED_EDGE('',*,*,#6857,.T.);
#8945=ORIENTED_EDGE('',*,*,#6858,.F.);
#8946=ORIENTED_EDGE('',*,*,#6859,.F.);
#8947=ORIENTED_EDGE('',*,*,#6860,.F.);
#8948=ORIENTED_EDGE('',*,*,#6861,.F.);
#8949=ORIENTED_EDGE('',*,*,#6862,.F.);
#8950=ORIENTED_EDGE('',*,*,#6853,.F.);
#8951=ORIENTED_EDGE('',*,*,#6833,.F.);
#8952=ORIENTED_EDGE('',*,*,#6850,.F.);
#8953=ORIENTED_EDGE('',*,*,#6852,.F.);
#8954=ORIENTED_EDGE('',*,*,#6843,.F.);
#8955=ORIENTED_EDGE('',*,*,#6847,.F.);
#8956=ORIENTED_EDGE('',*,*,#6839,.F.);
#8957=ORIENTED_EDGE('',*,*,#6835,.F.);
#8958=ORIENTED_EDGE('',*,*,#6863,.T.);
#8959=ORIENTED_EDGE('',*,*,#6864,.F.);
#8960=ORIENTED_EDGE('',*,*,#6865,.F.);
#8961=ORIENTED_EDGE('',*,*,#6866,.F.);
#8962=ORIENTED_EDGE('',*,*,#6867,.F.);
#8963=ORIENTED_EDGE('',*,*,#6868,.F.);
#8964=ORIENTED_EDGE('',*,*,#6869,.F.);
#8965=ORIENTED_EDGE('',*,*,#6870,.F.);
#8966=ORIENTED_EDGE('',*,*,#6857,.F.);
#8967=ORIENTED_EDGE('',*,*,#6871,.T.);
#8968=ORIENTED_EDGE('',*,*,#6872,.F.);
#8969=ORIENTED_EDGE('',*,*,#6873,.T.);
#8970=ORIENTED_EDGE('',*,*,#6874,.T.);
#8971=ORIENTED_EDGE('',*,*,#6875,.T.);
#8972=ORIENTED_EDGE('',*,*,#6876,.F.);
#8973=ORIENTED_EDGE('',*,*,#6854,.T.);
#8974=ORIENTED_EDGE('',*,*,#6862,.T.);
#8975=ORIENTED_EDGE('',*,*,#6876,.T.);
#8976=ORIENTED_EDGE('',*,*,#6877,.T.);
#8977=ORIENTED_EDGE('',*,*,#6878,.T.);
#8978=ORIENTED_EDGE('',*,*,#6855,.T.);
#8979=ORIENTED_EDGE('',*,*,#6879,.T.);
#8980=ORIENTED_EDGE('',*,*,#6880,.T.);
#8981=ORIENTED_EDGE('',*,*,#6881,.T.);
#8982=ORIENTED_EDGE('',*,*,#6882,.T.);
#8983=ORIENTED_EDGE('',*,*,#6879,.F.);
#8984=ORIENTED_EDGE('',*,*,#6883,.T.);
#8985=ORIENTED_EDGE('',*,*,#6878,.F.);
#8986=ORIENTED_EDGE('',*,*,#6884,.T.);
#8987=ORIENTED_EDGE('',*,*,#6872,.T.);
#8988=ORIENTED_EDGE('',*,*,#6885,.T.);
#8989=ORIENTED_EDGE('',*,*,#6886,.T.);
#8990=ORIENTED_EDGE('',*,*,#6887,.T.);
#8991=ORIENTED_EDGE('',*,*,#6886,.F.);
#8992=ORIENTED_EDGE('',*,*,#6888,.T.);
#8993=ORIENTED_EDGE('',*,*,#6881,.F.);
#8994=ORIENTED_EDGE('',*,*,#6889,.T.);
#8995=ORIENTED_EDGE('',*,*,#6851,.F.);
#8996=ORIENTED_EDGE('',*,*,#6856,.F.);
#8997=ORIENTED_EDGE('',*,*,#6883,.F.);
#8998=ORIENTED_EDGE('',*,*,#6882,.F.);
#8999=ORIENTED_EDGE('',*,*,#6888,.F.);
#9000=ORIENTED_EDGE('',*,*,#6890,.F.);
#9001=ORIENTED_EDGE('',*,*,#6891,.F.);
#9002=ORIENTED_EDGE('',*,*,#6892,.F.);
#9003=ORIENTED_EDGE('',*,*,#6893,.F.);
#9004=ORIENTED_EDGE('',*,*,#6894,.F.);
#9005=ORIENTED_EDGE('',*,*,#6846,.F.);
#9006=ORIENTED_EDGE('',*,*,#6845,.F.);
#9007=ORIENTED_EDGE('',*,*,#6895,.T.);
#9008=ORIENTED_EDGE('',*,*,#6896,.F.);
#9009=ORIENTED_EDGE('',*,*,#6897,.T.);
#9010=ORIENTED_EDGE('',*,*,#6860,.T.);
#9011=ORIENTED_EDGE('',*,*,#6898,.T.);
#9012=ORIENTED_EDGE('',*,*,#6899,.F.);
#9013=ORIENTED_EDGE('',*,*,#6900,.T.);
#9014=ORIENTED_EDGE('',*,*,#6901,.T.);
#9015=ORIENTED_EDGE('',*,*,#6899,.T.);
#9016=ORIENTED_EDGE('',*,*,#6902,.T.);
#9017=ORIENTED_EDGE('',*,*,#6903,.T.);
#9018=ORIENTED_EDGE('',*,*,#6904,.T.);
#9019=ORIENTED_EDGE('',*,*,#6905,.T.);
#9020=ORIENTED_EDGE('',*,*,#6906,.T.);
#9021=ORIENTED_EDGE('',*,*,#6907,.T.);
#9022=ORIENTED_EDGE('',*,*,#6908,.T.);
#9023=ORIENTED_EDGE('',*,*,#6907,.F.);
#9024=ORIENTED_EDGE('',*,*,#6909,.T.);
#9025=ORIENTED_EDGE('',*,*,#6903,.F.);
#9026=ORIENTED_EDGE('',*,*,#6910,.T.);
#9027=ORIENTED_EDGE('',*,*,#6896,.T.);
#9028=ORIENTED_EDGE('',*,*,#6911,.T.);
#9029=ORIENTED_EDGE('',*,*,#6912,.T.);
#9030=ORIENTED_EDGE('',*,*,#6913,.T.);
#9031=ORIENTED_EDGE('',*,*,#6912,.F.);
#9032=ORIENTED_EDGE('',*,*,#6914,.T.);
#9033=ORIENTED_EDGE('',*,*,#6905,.F.);
#9034=ORIENTED_EDGE('',*,*,#6915,.T.);
#9035=ORIENTED_EDGE('',*,*,#6911,.F.);
#9036=ORIENTED_EDGE('',*,*,#6895,.F.);
#9037=ORIENTED_EDGE('',*,*,#6859,.T.);
#9038=ORIENTED_EDGE('',*,*,#6916,.F.);
#9039=ORIENTED_EDGE('',*,*,#6917,.F.);
#9040=ORIENTED_EDGE('',*,*,#6918,.T.);
#9041=ORIENTED_EDGE('',*,*,#6875,.F.);
#9042=ORIENTED_EDGE('',*,*,#6861,.T.);
#9043=ORIENTED_EDGE('',*,*,#6897,.F.);
#9044=ORIENTED_EDGE('',*,*,#6913,.F.);
#9045=ORIENTED_EDGE('',*,*,#6915,.F.);
#9046=ORIENTED_EDGE('',*,*,#6908,.F.);
#9047=ORIENTED_EDGE('',*,*,#6910,.F.);
#9048=ORIENTED_EDGE('',*,*,#6902,.F.);
#9049=ORIENTED_EDGE('',*,*,#6898,.F.);
#9050=ORIENTED_EDGE('',*,*,#6919,.F.);
#9051=ORIENTED_EDGE('',*,*,#6873,.F.);
#9052=ORIENTED_EDGE('',*,*,#6887,.F.);
#9053=ORIENTED_EDGE('',*,*,#6889,.F.);
#9054=ORIENTED_EDGE('',*,*,#6880,.F.);
#9055=ORIENTED_EDGE('',*,*,#6884,.F.);
#9056=ORIENTED_EDGE('',*,*,#6877,.F.);
#9057=ORIENTED_EDGE('',*,*,#6920,.T.);
#9058=ORIENTED_EDGE('',*,*,#6921,.F.);
#9059=ORIENTED_EDGE('',*,*,#6864,.T.);
#9060=ORIENTED_EDGE('',*,*,#6922,.T.);
#9061=ORIENTED_EDGE('',*,*,#6870,.T.);
#9062=ORIENTED_EDGE('',*,*,#6923,.F.);
#9063=ORIENTED_EDGE('',*,*,#6916,.T.);
#9064=ORIENTED_EDGE('',*,*,#6858,.T.);
#9065=ORIENTED_EDGE('',*,*,#6923,.T.);
#9066=ORIENTED_EDGE('',*,*,#6869,.T.);
#9067=ORIENTED_EDGE('',*,*,#6924,.T.);
#9068=ORIENTED_EDGE('',*,*,#6917,.T.);
#9069=ORIENTED_EDGE('',*,*,#6925,.T.);
#9070=ORIENTED_EDGE('',*,*,#6926,.T.);
#9071=ORIENTED_EDGE('',*,*,#6927,.T.);
#9072=ORIENTED_EDGE('',*,*,#6867,.T.);
#9073=ORIENTED_EDGE('',*,*,#6927,.F.);
#9074=ORIENTED_EDGE('',*,*,#6928,.T.);
#9075=ORIENTED_EDGE('',*,*,#6924,.F.);
#9076=ORIENTED_EDGE('',*,*,#6868,.T.);
#9077=ORIENTED_EDGE('',*,*,#6921,.T.);
#9078=ORIENTED_EDGE('',*,*,#6929,.T.);
#9079=ORIENTED_EDGE('',*,*,#6930,.T.);
#9080=ORIENTED_EDGE('',*,*,#6865,.T.);
#9081=ORIENTED_EDGE('',*,*,#6930,.F.);
#9082=ORIENTED_EDGE('',*,*,#6931,.T.);
#9083=ORIENTED_EDGE('',*,*,#6925,.F.);
#9084=ORIENTED_EDGE('',*,*,#6866,.T.);
#9085=ORIENTED_EDGE('',*,*,#6914,.F.);
#9086=ORIENTED_EDGE('',*,*,#6918,.F.);
#9087=ORIENTED_EDGE('',*,*,#6928,.F.);
#9088=ORIENTED_EDGE('',*,*,#6926,.F.);
#9089=ORIENTED_EDGE('',*,*,#6931,.F.);
#9090=ORIENTED_EDGE('',*,*,#6932,.F.);
#9091=ORIENTED_EDGE('',*,*,#6933,.T.);
#9092=ORIENTED_EDGE('',*,*,#6934,.F.);
#9093=ORIENTED_EDGE('',*,*,#6935,.T.);
#9094=ORIENTED_EDGE('',*,*,#6936,.F.);
#9095=ORIENTED_EDGE('',*,*,#6909,.F.);
#9096=ORIENTED_EDGE('',*,*,#6906,.F.);
#9097=ORIENTED_EDGE('',*,*,#6920,.F.);
#9098=ORIENTED_EDGE('',*,*,#6937,.T.);
#9099=ORIENTED_EDGE('',*,*,#6938,.T.);
#9100=ORIENTED_EDGE('',*,*,#6932,.T.);
#9101=ORIENTED_EDGE('',*,*,#6929,.F.);
#9102=ORIENTED_EDGE('',*,*,#6938,.F.);
#9103=ORIENTED_EDGE('',*,*,#6939,.F.);
#9104=ORIENTED_EDGE('',*,*,#6940,.F.);
#9105=ORIENTED_EDGE('',*,*,#6893,.T.);
#9106=ORIENTED_EDGE('',*,*,#6941,.F.);
#9107=ORIENTED_EDGE('',*,*,#6942,.T.);
#9108=ORIENTED_EDGE('',*,*,#6943,.F.);
#9109=ORIENTED_EDGE('',*,*,#6933,.F.);
#9110=ORIENTED_EDGE('',*,*,#6838,.F.);
#9111=ORIENTED_EDGE('',*,*,#6944,.F.);
#9112=ORIENTED_EDGE('',*,*,#6939,.T.);
#9113=ORIENTED_EDGE('',*,*,#6937,.F.);
#9114=ORIENTED_EDGE('',*,*,#6922,.F.);
#9115=ORIENTED_EDGE('',*,*,#6863,.F.);
#9116=ORIENTED_EDGE('',*,*,#6841,.F.);
#9117=ORIENTED_EDGE('',*,*,#6894,.T.);
#9118=ORIENTED_EDGE('',*,*,#6940,.T.);
#9119=ORIENTED_EDGE('',*,*,#6944,.T.);
#9120=ORIENTED_EDGE('',*,*,#6837,.F.);
#9121=ORIENTED_EDGE('',*,*,#6945,.T.);
#9122=ORIENTED_EDGE('',*,*,#6934,.T.);
#9123=ORIENTED_EDGE('',*,*,#6943,.T.);
#9124=ORIENTED_EDGE('',*,*,#6946,.T.);
#9125=ORIENTED_EDGE('',*,*,#6945,.F.);
#9126=ORIENTED_EDGE('',*,*,#6947,.F.);
#9127=ORIENTED_EDGE('',*,*,#6948,.F.);
#9128=ORIENTED_EDGE('',*,*,#6891,.T.);
#9129=ORIENTED_EDGE('',*,*,#6949,.F.);
#9130=ORIENTED_EDGE('',*,*,#6950,.T.);
#9131=ORIENTED_EDGE('',*,*,#6951,.F.);
#9132=ORIENTED_EDGE('',*,*,#6935,.F.);
#9133=ORIENTED_EDGE('',*,*,#6946,.F.);
#9134=ORIENTED_EDGE('',*,*,#6942,.F.);
#9135=ORIENTED_EDGE('',*,*,#6952,.F.);
#9136=ORIENTED_EDGE('',*,*,#6947,.T.);
#9137=ORIENTED_EDGE('',*,*,#6948,.T.);
#9138=ORIENTED_EDGE('',*,*,#6952,.T.);
#9139=ORIENTED_EDGE('',*,*,#6941,.T.);
#9140=ORIENTED_EDGE('',*,*,#6892,.T.);
#9141=ORIENTED_EDGE('',*,*,#6904,.F.);
#9142=ORIENTED_EDGE('',*,*,#6936,.T.);
#9143=ORIENTED_EDGE('',*,*,#6951,.T.);
#9144=ORIENTED_EDGE('',*,*,#6953,.T.);
#9145=ORIENTED_EDGE('',*,*,#6900,.F.);
#9146=ORIENTED_EDGE('',*,*,#6874,.F.);
#9147=ORIENTED_EDGE('',*,*,#6919,.T.);
#9148=ORIENTED_EDGE('',*,*,#6901,.F.);
#9149=ORIENTED_EDGE('',*,*,#6953,.F.);
#9150=ORIENTED_EDGE('',*,*,#6950,.F.);
#9151=ORIENTED_EDGE('',*,*,#6954,.F.);
#9152=ORIENTED_EDGE('',*,*,#6871,.F.);
#9153=ORIENTED_EDGE('',*,*,#6954,.T.);
#9154=ORIENTED_EDGE('',*,*,#6949,.T.);
#9155=ORIENTED_EDGE('',*,*,#6890,.T.);
#9156=ORIENTED_EDGE('',*,*,#6885,.F.);
#9157=ORIENTED_EDGE('',*,*,#6955,.T.);
#9158=ORIENTED_EDGE('',*,*,#6956,.F.);
#9159=ORIENTED_EDGE('',*,*,#6957,.T.);
#9160=ORIENTED_EDGE('',*,*,#6958,.T.);
#9161=ORIENTED_EDGE('',*,*,#6959,.T.);
#9162=ORIENTED_EDGE('',*,*,#6960,.F.);
#9163=ORIENTED_EDGE('',*,*,#6961,.T.);
#9164=ORIENTED_EDGE('',*,*,#6962,.T.);
#9165=ORIENTED_EDGE('',*,*,#6960,.T.);
#9166=ORIENTED_EDGE('',*,*,#6963,.T.);
#9167=ORIENTED_EDGE('',*,*,#6964,.T.);
#9168=ORIENTED_EDGE('',*,*,#6965,.T.);
#9169=ORIENTED_EDGE('',*,*,#6966,.T.);
#9170=ORIENTED_EDGE('',*,*,#6967,.T.);
#9171=ORIENTED_EDGE('',*,*,#6964,.F.);
#9172=ORIENTED_EDGE('',*,*,#6968,.T.);
#9173=ORIENTED_EDGE('',*,*,#6956,.T.);
#9174=ORIENTED_EDGE('',*,*,#6969,.T.);
#9175=ORIENTED_EDGE('',*,*,#6966,.F.);
#9176=ORIENTED_EDGE('',*,*,#6970,.T.);
#9177=ORIENTED_EDGE('',*,*,#6957,.F.);
#9178=ORIENTED_EDGE('',*,*,#6970,.F.);
#9179=ORIENTED_EDGE('',*,*,#6971,.T.);
#9180=ORIENTED_EDGE('',*,*,#6972,.F.);
#9181=ORIENTED_EDGE('',*,*,#6973,.F.);
#9182=ORIENTED_EDGE('',*,*,#6974,.T.);
#9183=ORIENTED_EDGE('',*,*,#6968,.F.);
#9184=ORIENTED_EDGE('',*,*,#6975,.F.);
#9185=ORIENTED_EDGE('',*,*,#6976,.F.);
#9186=ORIENTED_EDGE('',*,*,#6971,.F.);
#9187=ORIENTED_EDGE('',*,*,#6963,.F.);
#9188=ORIENTED_EDGE('',*,*,#6959,.F.);
#9189=ORIENTED_EDGE('',*,*,#6977,.T.);
#9190=ORIENTED_EDGE('',*,*,#6978,.F.);
#9191=ORIENTED_EDGE('',*,*,#6979,.F.);
#9192=ORIENTED_EDGE('',*,*,#6975,.T.);
#9193=ORIENTED_EDGE('',*,*,#6962,.F.);
#9194=ORIENTED_EDGE('',*,*,#6980,.F.);
#9195=ORIENTED_EDGE('',*,*,#6981,.F.);
#9196=ORIENTED_EDGE('',*,*,#6982,.F.);
#9197=ORIENTED_EDGE('',*,*,#6983,.F.);
#9198=ORIENTED_EDGE('',*,*,#6984,.F.);
#9199=ORIENTED_EDGE('',*,*,#6985,.F.);
#9200=ORIENTED_EDGE('',*,*,#6977,.F.);
#9201=ORIENTED_EDGE('',*,*,#6973,.T.);
#9202=ORIENTED_EDGE('',*,*,#6986,.F.);
#9203=ORIENTED_EDGE('',*,*,#6987,.T.);
#9204=ORIENTED_EDGE('',*,*,#6988,.T.);
#9205=ORIENTED_EDGE('',*,*,#6989,.T.);
#9206=ORIENTED_EDGE('',*,*,#6990,.F.);
#9207=ORIENTED_EDGE('',*,*,#6978,.T.);
#9208=ORIENTED_EDGE('',*,*,#6985,.T.);
#9209=ORIENTED_EDGE('',*,*,#6990,.T.);
#9210=ORIENTED_EDGE('',*,*,#6991,.T.);
#9211=ORIENTED_EDGE('',*,*,#6992,.T.);
#9212=ORIENTED_EDGE('',*,*,#6979,.T.);
#9213=ORIENTED_EDGE('',*,*,#6993,.T.);
#9214=ORIENTED_EDGE('',*,*,#6976,.T.);
#9215=ORIENTED_EDGE('',*,*,#6992,.F.);
#9216=ORIENTED_EDGE('',*,*,#6994,.T.);
#9217=ORIENTED_EDGE('',*,*,#6986,.T.);
#9218=ORIENTED_EDGE('',*,*,#6972,.T.);
#9219=ORIENTED_EDGE('',*,*,#6993,.F.);
#9220=ORIENTED_EDGE('',*,*,#6995,.T.);
#9221=ORIENTED_EDGE('',*,*,#6987,.F.);
#9222=ORIENTED_EDGE('',*,*,#6995,.F.);
#9223=ORIENTED_EDGE('',*,*,#6996,.T.);
#9224=ORIENTED_EDGE('',*,*,#6997,.F.);
#9225=ORIENTED_EDGE('',*,*,#6998,.F.);
#9226=ORIENTED_EDGE('',*,*,#6999,.T.);
#9227=ORIENTED_EDGE('',*,*,#6994,.F.);
#9228=ORIENTED_EDGE('',*,*,#7000,.F.);
#9229=ORIENTED_EDGE('',*,*,#7001,.F.);
#9230=ORIENTED_EDGE('',*,*,#6996,.F.);
#9231=ORIENTED_EDGE('',*,*,#6991,.F.);
#9232=ORIENTED_EDGE('',*,*,#6989,.F.);
#9233=ORIENTED_EDGE('',*,*,#6984,.T.);
#9234=ORIENTED_EDGE('',*,*,#7002,.F.);
#9235=ORIENTED_EDGE('',*,*,#7003,.F.);
#9236=ORIENTED_EDGE('',*,*,#7000,.T.);
#9237=ORIENTED_EDGE('',*,*,#7004,.T.);
#9238=ORIENTED_EDGE('',*,*,#7005,.F.);
#9239=ORIENTED_EDGE('',*,*,#7002,.T.);
#9240=ORIENTED_EDGE('',*,*,#6983,.T.);
#9241=ORIENTED_EDGE('',*,*,#6998,.T.);
#9242=ORIENTED_EDGE('',*,*,#7006,.F.);
#9243=ORIENTED_EDGE('',*,*,#7007,.T.);
#9244=ORIENTED_EDGE('',*,*,#7008,.T.);
#9245=ORIENTED_EDGE('',*,*,#7006,.T.);
#9246=ORIENTED_EDGE('',*,*,#6997,.T.);
#9247=ORIENTED_EDGE('',*,*,#7009,.T.);
#9248=ORIENTED_EDGE('',*,*,#7010,.T.);
#9249=ORIENTED_EDGE('',*,*,#7009,.F.);
#9250=ORIENTED_EDGE('',*,*,#7001,.T.);
#9251=ORIENTED_EDGE('',*,*,#7011,.T.);
#9252=ORIENTED_EDGE('',*,*,#7012,.T.);
#9253=ORIENTED_EDGE('',*,*,#7005,.T.);
#9254=ORIENTED_EDGE('',*,*,#7013,.T.);
#9255=ORIENTED_EDGE('',*,*,#7011,.F.);
#9256=ORIENTED_EDGE('',*,*,#7003,.T.);
#9257=ORIENTED_EDGE('',*,*,#7014,.T.);
#9258=ORIENTED_EDGE('',*,*,#7015,.F.);
#9259=ORIENTED_EDGE('',*,*,#7016,.T.);
#9260=ORIENTED_EDGE('',*,*,#6981,.T.);
#9261=ORIENTED_EDGE('',*,*,#7017,.T.);
#9262=ORIENTED_EDGE('',*,*,#7018,.F.);
#9263=ORIENTED_EDGE('',*,*,#7019,.T.);
#9264=ORIENTED_EDGE('',*,*,#7020,.T.);
#9265=ORIENTED_EDGE('',*,*,#7018,.T.);
#9266=ORIENTED_EDGE('',*,*,#7021,.T.);
#9267=ORIENTED_EDGE('',*,*,#7022,.T.);
#9268=ORIENTED_EDGE('',*,*,#7023,.T.);
#9269=ORIENTED_EDGE('',*,*,#7022,.F.);
#9270=ORIENTED_EDGE('',*,*,#7024,.T.);
#9271=ORIENTED_EDGE('',*,*,#7025,.T.);
#9272=ORIENTED_EDGE('',*,*,#7026,.T.);
#9273=ORIENTED_EDGE('',*,*,#7015,.T.);
#9274=ORIENTED_EDGE('',*,*,#7027,.T.);
#9275=ORIENTED_EDGE('',*,*,#7025,.F.);
#9276=ORIENTED_EDGE('',*,*,#7028,.T.);
#9277=ORIENTED_EDGE('',*,*,#7004,.F.);
#9278=ORIENTED_EDGE('',*,*,#6982,.T.);
#9279=ORIENTED_EDGE('',*,*,#7016,.F.);
#9280=ORIENTED_EDGE('',*,*,#7028,.F.);
#9281=ORIENTED_EDGE('',*,*,#7029,.T.);
#9282=ORIENTED_EDGE('',*,*,#7013,.F.);
#9283=ORIENTED_EDGE('',*,*,#7012,.F.);
#9284=ORIENTED_EDGE('',*,*,#7029,.F.);
#9285=ORIENTED_EDGE('',*,*,#7024,.F.);
#9286=ORIENTED_EDGE('',*,*,#7030,.F.);
#9287=ORIENTED_EDGE('',*,*,#7010,.F.);
#9288=ORIENTED_EDGE('',*,*,#7030,.T.);
#9289=ORIENTED_EDGE('',*,*,#7021,.F.);
#9290=ORIENTED_EDGE('',*,*,#7017,.F.);
#9291=ORIENTED_EDGE('',*,*,#7031,.T.);
#9292=ORIENTED_EDGE('',*,*,#7007,.F.);
#9293=ORIENTED_EDGE('',*,*,#6955,.F.);
#9294=ORIENTED_EDGE('',*,*,#7032,.T.);
#9295=ORIENTED_EDGE('',*,*,#7019,.F.);
#9296=ORIENTED_EDGE('',*,*,#7023,.F.);
#9297=ORIENTED_EDGE('',*,*,#7033,.T.);
#9298=ORIENTED_EDGE('',*,*,#6969,.F.);
#9299=ORIENTED_EDGE('',*,*,#6958,.F.);
#9300=ORIENTED_EDGE('',*,*,#6974,.F.);
#9301=ORIENTED_EDGE('',*,*,#6988,.F.);
#9302=ORIENTED_EDGE('',*,*,#6999,.F.);
#9303=ORIENTED_EDGE('',*,*,#7008,.F.);
#9304=ORIENTED_EDGE('',*,*,#7031,.F.);
#9305=ORIENTED_EDGE('',*,*,#7020,.F.);
#9306=ORIENTED_EDGE('',*,*,#7032,.F.);
#9307=ORIENTED_EDGE('',*,*,#6965,.F.);
#9308=ORIENTED_EDGE('',*,*,#7034,.T.);
#9309=ORIENTED_EDGE('',*,*,#7027,.F.);
#9310=ORIENTED_EDGE('',*,*,#7014,.F.);
#9311=ORIENTED_EDGE('',*,*,#6980,.T.);
#9312=ORIENTED_EDGE('',*,*,#6961,.F.);
#9313=ORIENTED_EDGE('',*,*,#6967,.F.);
#9314=ORIENTED_EDGE('',*,*,#7033,.F.);
#9315=ORIENTED_EDGE('',*,*,#7026,.F.);
#9316=ORIENTED_EDGE('',*,*,#7034,.F.);
#9317=ORIENTED_EDGE('',*,*,#7035,.T.);
#9318=ORIENTED_EDGE('',*,*,#7036,.T.);
#9319=ORIENTED_EDGE('',*,*,#7037,.T.);
#9320=ORIENTED_EDGE('',*,*,#7036,.F.);
#9321=ORIENTED_EDGE('',*,*,#7037,.F.);
#9322=ORIENTED_EDGE('',*,*,#7038,.T.);
#9323=ORIENTED_EDGE('',*,*,#7039,.F.);
#9324=ORIENTED_EDGE('',*,*,#7038,.F.);
#9325=ORIENTED_EDGE('',*,*,#7040,.F.);
#9326=ORIENTED_EDGE('',*,*,#7041,.T.);
#9327=ORIENTED_EDGE('',*,*,#7042,.F.);
#9328=ORIENTED_EDGE('',*,*,#7043,.F.);
#9329=ORIENTED_EDGE('',*,*,#7035,.F.);
#9330=ORIENTED_EDGE('',*,*,#7044,.T.);
#9331=ORIENTED_EDGE('',*,*,#7045,.T.);
#9332=ORIENTED_EDGE('',*,*,#7039,.T.);
#9333=ORIENTED_EDGE('',*,*,#7045,.F.);
#9334=ORIENTED_EDGE('',*,*,#7046,.F.);
#9335=ORIENTED_EDGE('',*,*,#7047,.T.);
#9336=ORIENTED_EDGE('',*,*,#7048,.F.);
#9337=ORIENTED_EDGE('',*,*,#7049,.F.);
#9338=ORIENTED_EDGE('',*,*,#7044,.F.);
#9339=ORIENTED_EDGE('',*,*,#7050,.T.);
#9340=ORIENTED_EDGE('',*,*,#7051,.T.);
#9341=ORIENTED_EDGE('',*,*,#7052,.T.);
#9342=ORIENTED_EDGE('',*,*,#7053,.T.);
#9343=ORIENTED_EDGE('',*,*,#7054,.T.);
#9344=ORIENTED_EDGE('',*,*,#7055,.T.);
#9345=ORIENTED_EDGE('',*,*,#7050,.F.);
#9346=ORIENTED_EDGE('',*,*,#7056,.T.);
#9347=ORIENTED_EDGE('',*,*,#7057,.T.);
#9348=ORIENTED_EDGE('',*,*,#7058,.T.);
#9349=ORIENTED_EDGE('',*,*,#7054,.F.);
#9350=ORIENTED_EDGE('',*,*,#7059,.T.);
#9351=ORIENTED_EDGE('',*,*,#7060,.T.);
#9352=ORIENTED_EDGE('',*,*,#7061,.T.);
#9353=ORIENTED_EDGE('',*,*,#7057,.F.);
#9354=ORIENTED_EDGE('',*,*,#7062,.T.);
#9355=ORIENTED_EDGE('',*,*,#7063,.T.);
#9356=ORIENTED_EDGE('',*,*,#7064,.T.);
#9357=ORIENTED_EDGE('',*,*,#7060,.F.);
#9358=ORIENTED_EDGE('',*,*,#7046,.T.);
#9359=ORIENTED_EDGE('',*,*,#7065,.T.);
#9360=ORIENTED_EDGE('',*,*,#7066,.T.);
#9361=ORIENTED_EDGE('',*,*,#7063,.F.);
#9362=ORIENTED_EDGE('',*,*,#7067,.T.);
#9363=ORIENTED_EDGE('',*,*,#7068,.T.);
#9364=ORIENTED_EDGE('',*,*,#7069,.T.);
#9365=ORIENTED_EDGE('',*,*,#7065,.F.);
#9366=ORIENTED_EDGE('',*,*,#7070,.T.);
#9367=ORIENTED_EDGE('',*,*,#7052,.F.);
#9368=ORIENTED_EDGE('',*,*,#7071,.T.);
#9369=ORIENTED_EDGE('',*,*,#7068,.F.);
#9370=ORIENTED_EDGE('',*,*,#7072,.T.);
#9371=ORIENTED_EDGE('',*,*,#7062,.F.);
#9372=ORIENTED_EDGE('',*,*,#7073,.T.);
#9373=ORIENTED_EDGE('',*,*,#7074,.F.);
#9374=ORIENTED_EDGE('',*,*,#7047,.F.);
#9375=ORIENTED_EDGE('',*,*,#7059,.F.);
#9376=ORIENTED_EDGE('',*,*,#7075,.T.);
#9377=ORIENTED_EDGE('',*,*,#7076,.F.);
#9378=ORIENTED_EDGE('',*,*,#7073,.F.);
#9379=ORIENTED_EDGE('',*,*,#7056,.F.);
#9380=ORIENTED_EDGE('',*,*,#7077,.T.);
#9381=ORIENTED_EDGE('',*,*,#7078,.F.);
#9382=ORIENTED_EDGE('',*,*,#7075,.F.);
#9383=ORIENTED_EDGE('',*,*,#7053,.F.);
#9384=ORIENTED_EDGE('',*,*,#7079,.T.);
#9385=ORIENTED_EDGE('',*,*,#7080,.F.);
#9386=ORIENTED_EDGE('',*,*,#7077,.F.);
#9387=ORIENTED_EDGE('',*,*,#7081,.F.);
#9388=ORIENTED_EDGE('',*,*,#7082,.F.);
#9389=ORIENTED_EDGE('',*,*,#7083,.F.);
#9390=ORIENTED_EDGE('',*,*,#7084,.F.);
#9391=ORIENTED_EDGE('',*,*,#7085,.F.);
#9392=ORIENTED_EDGE('',*,*,#7086,.F.);
#9393=ORIENTED_EDGE('',*,*,#7087,.F.);
#9394=ORIENTED_EDGE('',*,*,#7088,.F.);
#9395=ORIENTED_EDGE('',*,*,#7051,.F.);
#9396=ORIENTED_EDGE('',*,*,#7055,.F.);
#9397=ORIENTED_EDGE('',*,*,#7058,.F.);
#9398=ORIENTED_EDGE('',*,*,#7061,.F.);
#9399=ORIENTED_EDGE('',*,*,#7064,.F.);
#9400=ORIENTED_EDGE('',*,*,#7066,.F.);
#9401=ORIENTED_EDGE('',*,*,#7069,.F.);
#9402=ORIENTED_EDGE('',*,*,#7071,.F.);
#9403=ORIENTED_EDGE('',*,*,#7089,.T.);
#9404=ORIENTED_EDGE('',*,*,#7081,.T.);
#9405=ORIENTED_EDGE('',*,*,#7090,.T.);
#9406=ORIENTED_EDGE('',*,*,#7091,.T.);
#9407=ORIENTED_EDGE('',*,*,#7089,.F.);
#9408=ORIENTED_EDGE('',*,*,#7092,.T.);
#9409=ORIENTED_EDGE('',*,*,#7093,.T.);
#9410=ORIENTED_EDGE('',*,*,#7082,.T.);
#9411=ORIENTED_EDGE('',*,*,#7094,.T.);
#9412=ORIENTED_EDGE('',*,*,#7083,.T.);
#9413=ORIENTED_EDGE('',*,*,#7093,.F.);
#9414=ORIENTED_EDGE('',*,*,#7095,.T.);
#9415=ORIENTED_EDGE('',*,*,#7094,.F.);
#9416=ORIENTED_EDGE('',*,*,#7096,.T.);
#9417=ORIENTED_EDGE('',*,*,#7097,.T.);
#9418=ORIENTED_EDGE('',*,*,#7084,.T.);
#9419=ORIENTED_EDGE('',*,*,#7098,.T.);
#9420=ORIENTED_EDGE('',*,*,#7085,.T.);
#9421=ORIENTED_EDGE('',*,*,#7097,.F.);
#9422=ORIENTED_EDGE('',*,*,#7099,.T.);
#9423=ORIENTED_EDGE('',*,*,#7098,.F.);
#9424=ORIENTED_EDGE('',*,*,#7100,.T.);
#9425=ORIENTED_EDGE('',*,*,#7101,.T.);
#9426=ORIENTED_EDGE('',*,*,#7086,.T.);
#9427=ORIENTED_EDGE('',*,*,#7102,.T.);
#9428=ORIENTED_EDGE('',*,*,#7087,.T.);
#9429=ORIENTED_EDGE('',*,*,#7101,.F.);
#9430=ORIENTED_EDGE('',*,*,#7103,.T.);
#9431=ORIENTED_EDGE('',*,*,#7102,.F.);
#9432=ORIENTED_EDGE('',*,*,#7040,.T.);
#9433=ORIENTED_EDGE('',*,*,#7090,.F.);
#9434=ORIENTED_EDGE('',*,*,#7088,.T.);
#9435=ORIENTED_EDGE('',*,*,#7096,.F.);
#9436=ORIENTED_EDGE('',*,*,#7104,.T.);
#9437=ORIENTED_EDGE('',*,*,#7105,.F.);
#9438=ORIENTED_EDGE('',*,*,#7106,.F.);
#9439=ORIENTED_EDGE('',*,*,#7095,.F.);
#9440=ORIENTED_EDGE('',*,*,#7107,.T.);
#9441=ORIENTED_EDGE('',*,*,#7108,.F.);
#9442=ORIENTED_EDGE('',*,*,#7104,.F.);
#9443=ORIENTED_EDGE('',*,*,#7092,.F.);
#9444=ORIENTED_EDGE('',*,*,#7109,.T.);
#9445=ORIENTED_EDGE('',*,*,#7110,.F.);
#9446=ORIENTED_EDGE('',*,*,#7107,.F.);
#9447=ORIENTED_EDGE('',*,*,#7091,.F.);
#9448=ORIENTED_EDGE('',*,*,#7043,.T.);
#9449=ORIENTED_EDGE('',*,*,#7111,.F.);
#9450=ORIENTED_EDGE('',*,*,#7109,.F.);
#9451=ORIENTED_EDGE('',*,*,#7112,.T.);
#9452=ORIENTED_EDGE('',*,*,#7113,.T.);
#9453=ORIENTED_EDGE('',*,*,#7114,.T.);
#9454=ORIENTED_EDGE('',*,*,#7105,.T.);
#9455=ORIENTED_EDGE('',*,*,#7115,.T.);
#9456=ORIENTED_EDGE('',*,*,#7116,.T.);
#9457=ORIENTED_EDGE('',*,*,#7112,.F.);
#9458=ORIENTED_EDGE('',*,*,#7108,.T.);
#9459=ORIENTED_EDGE('',*,*,#7117,.T.);
#9460=ORIENTED_EDGE('',*,*,#7118,.T.);
#9461=ORIENTED_EDGE('',*,*,#7115,.F.);
#9462=ORIENTED_EDGE('',*,*,#7110,.T.);
#9463=ORIENTED_EDGE('',*,*,#7119,.T.);
#9464=ORIENTED_EDGE('',*,*,#7120,.T.);
#9465=ORIENTED_EDGE('',*,*,#7117,.F.);
#9466=ORIENTED_EDGE('',*,*,#7111,.T.);
#9467=ORIENTED_EDGE('',*,*,#7121,.T.);
#9468=ORIENTED_EDGE('',*,*,#7122,.T.);
#9469=ORIENTED_EDGE('',*,*,#7119,.F.);
#9470=ORIENTED_EDGE('',*,*,#7042,.T.);
#9471=ORIENTED_EDGE('',*,*,#7123,.T.);
#9472=ORIENTED_EDGE('',*,*,#7124,.T.);
#9473=ORIENTED_EDGE('',*,*,#7121,.F.);
#9474=ORIENTED_EDGE('',*,*,#7125,.T.);
#9475=ORIENTED_EDGE('',*,*,#7126,.T.);
#9476=ORIENTED_EDGE('',*,*,#7127,.T.);
#9477=ORIENTED_EDGE('',*,*,#7123,.F.);
#9478=ORIENTED_EDGE('',*,*,#7128,.T.);
#9479=ORIENTED_EDGE('',*,*,#7114,.F.);
#9480=ORIENTED_EDGE('',*,*,#7129,.T.);
#9481=ORIENTED_EDGE('',*,*,#7126,.F.);
#9482=ORIENTED_EDGE('',*,*,#7130,.T.);
#9483=ORIENTED_EDGE('',*,*,#7113,.F.);
#9484=ORIENTED_EDGE('',*,*,#7116,.F.);
#9485=ORIENTED_EDGE('',*,*,#7118,.F.);
#9486=ORIENTED_EDGE('',*,*,#7120,.F.);
#9487=ORIENTED_EDGE('',*,*,#7122,.F.);
#9488=ORIENTED_EDGE('',*,*,#7124,.F.);
#9489=ORIENTED_EDGE('',*,*,#7127,.F.);
#9490=ORIENTED_EDGE('',*,*,#7129,.F.);
#9491=ORIENTED_EDGE('',*,*,#7131,.F.);
#9492=ORIENTED_EDGE('',*,*,#7132,.F.);
#9493=ORIENTED_EDGE('',*,*,#7133,.F.);
#9494=ORIENTED_EDGE('',*,*,#7134,.F.);
#9495=ORIENTED_EDGE('',*,*,#7135,.F.);
#9496=ORIENTED_EDGE('',*,*,#7136,.F.);
#9497=ORIENTED_EDGE('',*,*,#7137,.F.);
#9498=ORIENTED_EDGE('',*,*,#7138,.F.);
#9499=ORIENTED_EDGE('',*,*,#7139,.T.);
#9500=ORIENTED_EDGE('',*,*,#7131,.T.);
#9501=ORIENTED_EDGE('',*,*,#7140,.T.);
#9502=ORIENTED_EDGE('',*,*,#7076,.T.);
#9503=ORIENTED_EDGE('',*,*,#7141,.T.);
#9504=ORIENTED_EDGE('',*,*,#7132,.T.);
#9505=ORIENTED_EDGE('',*,*,#7139,.F.);
#9506=ORIENTED_EDGE('',*,*,#7078,.T.);
#9507=ORIENTED_EDGE('',*,*,#7142,.T.);
#9508=ORIENTED_EDGE('',*,*,#7133,.T.);
#9509=ORIENTED_EDGE('',*,*,#7141,.F.);
#9510=ORIENTED_EDGE('',*,*,#7080,.T.);
#9511=ORIENTED_EDGE('',*,*,#7143,.T.);
#9512=ORIENTED_EDGE('',*,*,#7134,.T.);
#9513=ORIENTED_EDGE('',*,*,#7142,.F.);
#9514=ORIENTED_EDGE('',*,*,#7144,.T.);
#9515=ORIENTED_EDGE('',*,*,#7145,.T.);
#9516=ORIENTED_EDGE('',*,*,#7135,.T.);
#9517=ORIENTED_EDGE('',*,*,#7143,.F.);
#9518=ORIENTED_EDGE('',*,*,#7146,.T.);
#9519=ORIENTED_EDGE('',*,*,#7147,.T.);
#9520=ORIENTED_EDGE('',*,*,#7136,.T.);
#9521=ORIENTED_EDGE('',*,*,#7145,.F.);
#9522=ORIENTED_EDGE('',*,*,#7148,.T.);
#9523=ORIENTED_EDGE('',*,*,#7149,.T.);
#9524=ORIENTED_EDGE('',*,*,#7137,.T.);
#9525=ORIENTED_EDGE('',*,*,#7147,.F.);
#9526=ORIENTED_EDGE('',*,*,#7048,.T.);
#9527=ORIENTED_EDGE('',*,*,#7140,.F.);
#9528=ORIENTED_EDGE('',*,*,#7138,.T.);
#9529=ORIENTED_EDGE('',*,*,#7149,.F.);
#9530=ORIENTED_EDGE('',*,*,#7074,.T.);
#9531=ORIENTED_EDGE('',*,*,#7072,.F.);
#9532=ORIENTED_EDGE('',*,*,#7150,.T.);
#9533=ORIENTED_EDGE('',*,*,#7144,.F.);
#9534=ORIENTED_EDGE('',*,*,#7079,.F.);
#9535=ORIENTED_EDGE('',*,*,#7067,.F.);
#9536=ORIENTED_EDGE('',*,*,#7049,.T.);
#9537=ORIENTED_EDGE('',*,*,#7148,.F.);
#9538=ORIENTED_EDGE('',*,*,#7151,.F.);
#9539=ORIENTED_EDGE('',*,*,#7070,.F.);
#9540=ORIENTED_EDGE('',*,*,#7151,.T.);
#9541=ORIENTED_EDGE('',*,*,#7146,.F.);
#9542=ORIENTED_EDGE('',*,*,#7150,.F.);
#9543=ORIENTED_EDGE('',*,*,#7099,.F.);
#9544=ORIENTED_EDGE('',*,*,#7106,.T.);
#9545=ORIENTED_EDGE('',*,*,#7130,.F.);
#9546=ORIENTED_EDGE('',*,*,#7152,.F.);
#9547=ORIENTED_EDGE('',*,*,#7100,.F.);
#9548=ORIENTED_EDGE('',*,*,#7152,.T.);
#9549=ORIENTED_EDGE('',*,*,#7128,.F.);
#9550=ORIENTED_EDGE('',*,*,#7153,.F.);
#9551=ORIENTED_EDGE('',*,*,#7103,.F.);
#9552=ORIENTED_EDGE('',*,*,#7153,.T.);
#9553=ORIENTED_EDGE('',*,*,#7125,.F.);
#9554=ORIENTED_EDGE('',*,*,#7041,.F.);
#9555=ORIENTED_EDGE('',*,*,#7154,.T.);
#9556=ORIENTED_EDGE('',*,*,#7155,.T.);
#9557=ORIENTED_EDGE('',*,*,#7156,.T.);
#9558=ORIENTED_EDGE('',*,*,#7155,.F.);
#9559=ORIENTED_EDGE('',*,*,#7157,.F.);
#9560=ORIENTED_EDGE('',*,*,#7158,.T.);
#9561=ORIENTED_EDGE('',*,*,#7159,.F.);
#9562=ORIENTED_EDGE('',*,*,#7160,.F.);
#9563=ORIENTED_EDGE('',*,*,#7161,.F.);
#9564=ORIENTED_EDGE('',*,*,#7162,.F.);
#9565=ORIENTED_EDGE('',*,*,#7163,.F.);
#9566=ORIENTED_EDGE('',*,*,#7164,.F.);
#9567=ORIENTED_EDGE('',*,*,#7165,.F.);
#9568=ORIENTED_EDGE('',*,*,#7154,.F.);
#9569=ORIENTED_EDGE('',*,*,#7166,.F.);
#9570=ORIENTED_EDGE('',*,*,#7167,.T.);
#9571=ORIENTED_EDGE('',*,*,#7156,.F.);
#9572=ORIENTED_EDGE('',*,*,#7167,.F.);
#9573=ORIENTED_EDGE('',*,*,#7161,.T.);
#9574=ORIENTED_EDGE('',*,*,#7168,.T.);
#9575=ORIENTED_EDGE('',*,*,#7169,.T.);
#9576=ORIENTED_EDGE('',*,*,#7168,.F.);
#9577=ORIENTED_EDGE('',*,*,#7170,.F.);
#9578=ORIENTED_EDGE('',*,*,#7171,.T.);
#9579=ORIENTED_EDGE('',*,*,#7169,.F.);
#9580=ORIENTED_EDGE('',*,*,#7171,.F.);
#9581=ORIENTED_EDGE('',*,*,#7165,.T.);
#9582=ORIENTED_EDGE('',*,*,#7172,.T.);
#9583=ORIENTED_EDGE('',*,*,#7173,.T.);
#9584=ORIENTED_EDGE('',*,*,#7172,.F.);
#9585=ORIENTED_EDGE('',*,*,#7174,.F.);
#9586=ORIENTED_EDGE('',*,*,#7175,.T.);
#9587=ORIENTED_EDGE('',*,*,#7173,.F.);
#9588=ORIENTED_EDGE('',*,*,#7175,.F.);
#9589=ORIENTED_EDGE('',*,*,#7162,.T.);
#9590=ORIENTED_EDGE('',*,*,#7176,.T.);
#9591=ORIENTED_EDGE('',*,*,#7177,.T.);
#9592=ORIENTED_EDGE('',*,*,#7176,.F.);
#9593=ORIENTED_EDGE('',*,*,#7178,.F.);
#9594=ORIENTED_EDGE('',*,*,#7179,.T.);
#9595=ORIENTED_EDGE('',*,*,#7177,.F.);
#9596=ORIENTED_EDGE('',*,*,#7179,.F.);
#9597=ORIENTED_EDGE('',*,*,#7164,.T.);
#9598=ORIENTED_EDGE('',*,*,#7180,.T.);
#9599=ORIENTED_EDGE('',*,*,#7181,.T.);
#9600=ORIENTED_EDGE('',*,*,#7180,.F.);
#9601=ORIENTED_EDGE('',*,*,#7182,.F.);
#9602=ORIENTED_EDGE('',*,*,#7183,.T.);
#9603=ORIENTED_EDGE('',*,*,#7181,.F.);
#9604=ORIENTED_EDGE('',*,*,#7183,.F.);
#9605=ORIENTED_EDGE('',*,*,#7163,.T.);
#9606=ORIENTED_EDGE('',*,*,#7184,.T.);
#9607=ORIENTED_EDGE('',*,*,#7185,.T.);
#9608=ORIENTED_EDGE('',*,*,#7184,.F.);
#9609=ORIENTED_EDGE('',*,*,#7186,.F.);
#9610=ORIENTED_EDGE('',*,*,#7187,.T.);
#9611=ORIENTED_EDGE('',*,*,#7185,.F.);
#9612=ORIENTED_EDGE('',*,*,#7187,.F.);
#9613=ORIENTED_EDGE('',*,*,#7188,.T.);
#9614=ORIENTED_EDGE('',*,*,#7189,.T.);
#9615=ORIENTED_EDGE('',*,*,#7190,.T.);
#9616=ORIENTED_EDGE('',*,*,#7189,.F.);
#9617=ORIENTED_EDGE('',*,*,#7191,.F.);
#9618=ORIENTED_EDGE('',*,*,#7192,.T.);
#9619=ORIENTED_EDGE('',*,*,#7193,.F.);
#9620=ORIENTED_EDGE('',*,*,#7194,.F.);
#9621=ORIENTED_EDGE('',*,*,#7195,.F.);
#9622=ORIENTED_EDGE('',*,*,#7196,.F.);
#9623=ORIENTED_EDGE('',*,*,#7197,.F.);
#9624=ORIENTED_EDGE('',*,*,#7198,.F.);
#9625=ORIENTED_EDGE('',*,*,#7199,.F.);
#9626=ORIENTED_EDGE('',*,*,#7200,.F.);
#9627=ORIENTED_EDGE('',*,*,#7188,.F.);
#9628=ORIENTED_EDGE('',*,*,#7201,.F.);
#9629=ORIENTED_EDGE('',*,*,#7202,.T.);
#9630=ORIENTED_EDGE('',*,*,#7190,.F.);
#9631=ORIENTED_EDGE('',*,*,#7202,.F.);
#9632=ORIENTED_EDGE('',*,*,#7203,.T.);
#9633=ORIENTED_EDGE('',*,*,#7191,.T.);
#9634=ORIENTED_EDGE('',*,*,#7204,.T.);
#9635=ORIENTED_EDGE('',*,*,#7205,.T.);
#9636=ORIENTED_EDGE('',*,*,#7206,.T.);
#9637=ORIENTED_EDGE('',*,*,#7207,.T.);
#9638=ORIENTED_EDGE('',*,*,#7203,.F.);
#9639=ORIENTED_EDGE('',*,*,#7208,.T.);
#9640=ORIENTED_EDGE('',*,*,#7209,.T.);
#9641=ORIENTED_EDGE('',*,*,#7210,.T.);
#9642=ORIENTED_EDGE('',*,*,#7206,.F.);
#9643=ORIENTED_EDGE('',*,*,#7211,.T.);
#9644=ORIENTED_EDGE('',*,*,#7212,.T.);
#9645=ORIENTED_EDGE('',*,*,#7213,.T.);
#9646=ORIENTED_EDGE('',*,*,#7209,.F.);
#9647=ORIENTED_EDGE('',*,*,#7214,.T.);
#9648=ORIENTED_EDGE('',*,*,#7215,.T.);
#9649=ORIENTED_EDGE('',*,*,#7216,.T.);
#9650=ORIENTED_EDGE('',*,*,#7212,.F.);
#9651=ORIENTED_EDGE('',*,*,#7217,.T.);
#9652=ORIENTED_EDGE('',*,*,#7218,.T.);
#9653=ORIENTED_EDGE('',*,*,#7219,.T.);
#9654=ORIENTED_EDGE('',*,*,#7215,.F.);
#9655=ORIENTED_EDGE('',*,*,#7220,.T.);
#9656=ORIENTED_EDGE('',*,*,#7221,.T.);
#9657=ORIENTED_EDGE('',*,*,#7157,.T.);
#9658=ORIENTED_EDGE('',*,*,#7218,.F.);
#9659=ORIENTED_EDGE('',*,*,#7222,.T.);
#9660=ORIENTED_EDGE('',*,*,#7204,.F.);
#9661=ORIENTED_EDGE('',*,*,#7223,.T.);
#9662=ORIENTED_EDGE('',*,*,#7221,.F.);
#9663=ORIENTED_EDGE('',*,*,#7224,.T.);
#9664=ORIENTED_EDGE('',*,*,#7219,.F.);
#9665=ORIENTED_EDGE('',*,*,#7160,.T.);
#9666=ORIENTED_EDGE('',*,*,#7225,.F.);
#9667=ORIENTED_EDGE('',*,*,#7226,.F.);
#9668=ORIENTED_EDGE('',*,*,#7223,.F.);
#9669=ORIENTED_EDGE('',*,*,#7194,.T.);
#9670=ORIENTED_EDGE('',*,*,#7227,.F.);
#9671=ORIENTED_EDGE('',*,*,#7158,.F.);
#9672=ORIENTED_EDGE('',*,*,#7228,.F.);
#9673=ORIENTED_EDGE('',*,*,#7229,.F.);
#9674=ORIENTED_EDGE('',*,*,#7230,.F.);
#9675=ORIENTED_EDGE('',*,*,#7231,.F.);
#9676=ORIENTED_EDGE('',*,*,#7232,.F.);
#9677=ORIENTED_EDGE('',*,*,#7233,.F.);
#9678=ORIENTED_EDGE('',*,*,#7234,.F.);
#9679=ORIENTED_EDGE('',*,*,#7235,.F.);
#9680=ORIENTED_EDGE('',*,*,#7205,.F.);
#9681=ORIENTED_EDGE('',*,*,#7224,.F.);
#9682=ORIENTED_EDGE('',*,*,#7222,.F.);
#9683=ORIENTED_EDGE('',*,*,#7220,.F.);
#9684=ORIENTED_EDGE('',*,*,#7217,.F.);
#9685=ORIENTED_EDGE('',*,*,#7214,.F.);
#9686=ORIENTED_EDGE('',*,*,#7211,.F.);
#9687=ORIENTED_EDGE('',*,*,#7208,.F.);
#9688=ORIENTED_EDGE('',*,*,#7200,.T.);
#9689=ORIENTED_EDGE('',*,*,#7236,.T.);
#9690=ORIENTED_EDGE('',*,*,#7237,.T.);
#9691=ORIENTED_EDGE('',*,*,#7236,.F.);
#9692=ORIENTED_EDGE('',*,*,#7238,.F.);
#9693=ORIENTED_EDGE('',*,*,#7239,.T.);
#9694=ORIENTED_EDGE('',*,*,#7237,.F.);
#9695=ORIENTED_EDGE('',*,*,#7239,.F.);
#9696=ORIENTED_EDGE('',*,*,#7195,.T.);
#9697=ORIENTED_EDGE('',*,*,#7240,.T.);
#9698=ORIENTED_EDGE('',*,*,#7241,.T.);
#9699=ORIENTED_EDGE('',*,*,#7240,.F.);
#9700=ORIENTED_EDGE('',*,*,#7242,.F.);
#9701=ORIENTED_EDGE('',*,*,#7243,.T.);
#9702=ORIENTED_EDGE('',*,*,#7241,.F.);
#9703=ORIENTED_EDGE('',*,*,#7243,.F.);
#9704=ORIENTED_EDGE('',*,*,#7199,.T.);
#9705=ORIENTED_EDGE('',*,*,#7244,.T.);
#9706=ORIENTED_EDGE('',*,*,#7245,.T.);
#9707=ORIENTED_EDGE('',*,*,#7244,.F.);
#9708=ORIENTED_EDGE('',*,*,#7246,.F.);
#9709=ORIENTED_EDGE('',*,*,#7247,.T.);
#9710=ORIENTED_EDGE('',*,*,#7245,.F.);
#9711=ORIENTED_EDGE('',*,*,#7247,.F.);
#9712=ORIENTED_EDGE('',*,*,#7196,.T.);
#9713=ORIENTED_EDGE('',*,*,#7248,.T.);
#9714=ORIENTED_EDGE('',*,*,#7249,.T.);
#9715=ORIENTED_EDGE('',*,*,#7248,.F.);
#9716=ORIENTED_EDGE('',*,*,#7250,.F.);
#9717=ORIENTED_EDGE('',*,*,#7251,.T.);
#9718=ORIENTED_EDGE('',*,*,#7249,.F.);
#9719=ORIENTED_EDGE('',*,*,#7251,.F.);
#9720=ORIENTED_EDGE('',*,*,#7198,.T.);
#9721=ORIENTED_EDGE('',*,*,#7252,.T.);
#9722=ORIENTED_EDGE('',*,*,#7253,.T.);
#9723=ORIENTED_EDGE('',*,*,#7252,.F.);
#9724=ORIENTED_EDGE('',*,*,#7254,.F.);
#9725=ORIENTED_EDGE('',*,*,#7255,.T.);
#9726=ORIENTED_EDGE('',*,*,#7253,.F.);
#9727=ORIENTED_EDGE('',*,*,#7255,.F.);
#9728=ORIENTED_EDGE('',*,*,#7197,.T.);
#9729=ORIENTED_EDGE('',*,*,#7256,.T.);
#9730=ORIENTED_EDGE('',*,*,#7257,.T.);
#9731=ORIENTED_EDGE('',*,*,#7256,.F.);
#9732=ORIENTED_EDGE('',*,*,#7258,.F.);
#9733=ORIENTED_EDGE('',*,*,#7259,.T.);
#9734=ORIENTED_EDGE('',*,*,#7257,.F.);
#9735=ORIENTED_EDGE('',*,*,#7259,.F.);
#9736=ORIENTED_EDGE('',*,*,#7260,.T.);
#9737=ORIENTED_EDGE('',*,*,#7261,.T.);
#9738=ORIENTED_EDGE('',*,*,#7238,.T.);
#9739=ORIENTED_EDGE('',*,*,#7261,.F.);
#9740=ORIENTED_EDGE('',*,*,#7262,.F.);
#9741=ORIENTED_EDGE('',*,*,#7263,.T.);
#9742=ORIENTED_EDGE('',*,*,#7264,.F.);
#9743=ORIENTED_EDGE('',*,*,#7265,.F.);
#9744=ORIENTED_EDGE('',*,*,#7266,.F.);
#9745=ORIENTED_EDGE('',*,*,#7267,.F.);
#9746=ORIENTED_EDGE('',*,*,#7268,.F.);
#9747=ORIENTED_EDGE('',*,*,#7269,.F.);
#9748=ORIENTED_EDGE('',*,*,#7270,.F.);
#9749=ORIENTED_EDGE('',*,*,#7271,.F.);
#9750=ORIENTED_EDGE('',*,*,#7260,.F.);
#9751=ORIENTED_EDGE('',*,*,#7266,.T.);
#9752=ORIENTED_EDGE('',*,*,#7272,.T.);
#9753=ORIENTED_EDGE('',*,*,#7201,.T.);
#9754=ORIENTED_EDGE('',*,*,#7272,.F.);
#9755=ORIENTED_EDGE('',*,*,#7271,.T.);
#9756=ORIENTED_EDGE('',*,*,#7273,.T.);
#9757=ORIENTED_EDGE('',*,*,#7242,.T.);
#9758=ORIENTED_EDGE('',*,*,#7273,.F.);
#9759=ORIENTED_EDGE('',*,*,#7267,.T.);
#9760=ORIENTED_EDGE('',*,*,#7274,.T.);
#9761=ORIENTED_EDGE('',*,*,#7246,.T.);
#9762=ORIENTED_EDGE('',*,*,#7274,.F.);
#9763=ORIENTED_EDGE('',*,*,#7270,.T.);
#9764=ORIENTED_EDGE('',*,*,#7275,.T.);
#9765=ORIENTED_EDGE('',*,*,#7250,.T.);
#9766=ORIENTED_EDGE('',*,*,#7275,.F.);
#9767=ORIENTED_EDGE('',*,*,#7268,.T.);
#9768=ORIENTED_EDGE('',*,*,#7276,.T.);
#9769=ORIENTED_EDGE('',*,*,#7254,.T.);
#9770=ORIENTED_EDGE('',*,*,#7276,.F.);
#9771=ORIENTED_EDGE('',*,*,#7269,.T.);
#9772=ORIENTED_EDGE('',*,*,#7277,.T.);
#9773=ORIENTED_EDGE('',*,*,#7258,.T.);
#9774=ORIENTED_EDGE('',*,*,#7277,.F.);
#9775=ORIENTED_EDGE('',*,*,#7278,.T.);
#9776=ORIENTED_EDGE('',*,*,#7279,.T.);
#9777=ORIENTED_EDGE('',*,*,#7280,.T.);
#9778=ORIENTED_EDGE('',*,*,#7228,.T.);
#9779=ORIENTED_EDGE('',*,*,#7281,.T.);
#9780=ORIENTED_EDGE('',*,*,#7282,.T.);
#9781=ORIENTED_EDGE('',*,*,#7278,.F.);
#9782=ORIENTED_EDGE('',*,*,#7235,.T.);
#9783=ORIENTED_EDGE('',*,*,#7283,.T.);
#9784=ORIENTED_EDGE('',*,*,#7284,.T.);
#9785=ORIENTED_EDGE('',*,*,#7281,.F.);
#9786=ORIENTED_EDGE('',*,*,#7234,.T.);
#9787=ORIENTED_EDGE('',*,*,#7285,.T.);
#9788=ORIENTED_EDGE('',*,*,#7286,.T.);
#9789=ORIENTED_EDGE('',*,*,#7283,.F.);
#9790=ORIENTED_EDGE('',*,*,#7233,.T.);
#9791=ORIENTED_EDGE('',*,*,#7287,.T.);
#9792=ORIENTED_EDGE('',*,*,#7288,.T.);
#9793=ORIENTED_EDGE('',*,*,#7285,.F.);
#9794=ORIENTED_EDGE('',*,*,#7232,.T.);
#9795=ORIENTED_EDGE('',*,*,#7289,.T.);
#9796=ORIENTED_EDGE('',*,*,#7290,.T.);
#9797=ORIENTED_EDGE('',*,*,#7287,.F.);
#9798=ORIENTED_EDGE('',*,*,#7231,.T.);
#9799=ORIENTED_EDGE('',*,*,#7291,.T.);
#9800=ORIENTED_EDGE('',*,*,#7262,.T.);
#9801=ORIENTED_EDGE('',*,*,#7289,.F.);
#9802=ORIENTED_EDGE('',*,*,#7230,.T.);
#9803=ORIENTED_EDGE('',*,*,#7280,.F.);
#9804=ORIENTED_EDGE('',*,*,#7292,.T.);
#9805=ORIENTED_EDGE('',*,*,#7291,.F.);
#9806=ORIENTED_EDGE('',*,*,#7229,.T.);
#9807=ORIENTED_EDGE('',*,*,#7290,.F.);
#9808=ORIENTED_EDGE('',*,*,#7265,.T.);
#9809=ORIENTED_EDGE('',*,*,#7293,.F.);
#9810=ORIENTED_EDGE('',*,*,#7294,.F.);
#9811=ORIENTED_EDGE('',*,*,#7292,.F.);
#9812=ORIENTED_EDGE('',*,*,#7295,.T.);
#9813=ORIENTED_EDGE('',*,*,#7296,.F.);
#9814=ORIENTED_EDGE('',*,*,#7263,.F.);
#9815=ORIENTED_EDGE('',*,*,#7279,.F.);
#9816=ORIENTED_EDGE('',*,*,#7297,.T.);
#9817=ORIENTED_EDGE('',*,*,#7298,.F.);
#9818=ORIENTED_EDGE('',*,*,#7295,.F.);
#9819=ORIENTED_EDGE('',*,*,#7299,.F.);
#9820=ORIENTED_EDGE('',*,*,#7300,.F.);
#9821=ORIENTED_EDGE('',*,*,#7301,.F.);
#9822=ORIENTED_EDGE('',*,*,#7302,.F.);
#9823=ORIENTED_EDGE('',*,*,#7303,.F.);
#9824=ORIENTED_EDGE('',*,*,#7304,.F.);
#9825=ORIENTED_EDGE('',*,*,#7299,.T.);
#9826=ORIENTED_EDGE('',*,*,#7305,.T.);
#9827=ORIENTED_EDGE('',*,*,#7186,.T.);
#9828=ORIENTED_EDGE('',*,*,#7305,.F.);
#9829=ORIENTED_EDGE('',*,*,#7304,.T.);
#9830=ORIENTED_EDGE('',*,*,#7306,.T.);
#9831=ORIENTED_EDGE('',*,*,#7182,.T.);
#9832=ORIENTED_EDGE('',*,*,#7306,.F.);
#9833=ORIENTED_EDGE('',*,*,#7300,.T.);
#9834=ORIENTED_EDGE('',*,*,#7307,.T.);
#9835=ORIENTED_EDGE('',*,*,#7178,.T.);
#9836=ORIENTED_EDGE('',*,*,#7307,.F.);
#9837=ORIENTED_EDGE('',*,*,#7303,.T.);
#9838=ORIENTED_EDGE('',*,*,#7308,.T.);
#9839=ORIENTED_EDGE('',*,*,#7174,.T.);
#9840=ORIENTED_EDGE('',*,*,#7308,.F.);
#9841=ORIENTED_EDGE('',*,*,#7301,.T.);
#9842=ORIENTED_EDGE('',*,*,#7309,.T.);
#9843=ORIENTED_EDGE('',*,*,#7170,.T.);
#9844=ORIENTED_EDGE('',*,*,#7309,.F.);
#9845=ORIENTED_EDGE('',*,*,#7302,.T.);
#9846=ORIENTED_EDGE('',*,*,#7310,.T.);
#9847=ORIENTED_EDGE('',*,*,#7166,.T.);
#9848=ORIENTED_EDGE('',*,*,#7310,.F.);
#9849=ORIENTED_EDGE('',*,*,#7311,.T.);
#9850=ORIENTED_EDGE('',*,*,#7312,.T.);
#9851=ORIENTED_EDGE('',*,*,#7313,.T.);
#9852=ORIENTED_EDGE('',*,*,#7264,.T.);
#9853=ORIENTED_EDGE('',*,*,#7314,.T.);
#9854=ORIENTED_EDGE('',*,*,#7315,.T.);
#9855=ORIENTED_EDGE('',*,*,#7311,.F.);
#9856=ORIENTED_EDGE('',*,*,#7296,.T.);
#9857=ORIENTED_EDGE('',*,*,#7316,.T.);
#9858=ORIENTED_EDGE('',*,*,#7317,.T.);
#9859=ORIENTED_EDGE('',*,*,#7314,.F.);
#9860=ORIENTED_EDGE('',*,*,#7298,.T.);
#9861=ORIENTED_EDGE('',*,*,#7318,.T.);
#9862=ORIENTED_EDGE('',*,*,#7319,.T.);
#9863=ORIENTED_EDGE('',*,*,#7316,.F.);
#9864=ORIENTED_EDGE('',*,*,#7320,.T.);
#9865=ORIENTED_EDGE('',*,*,#7321,.T.);
#9866=ORIENTED_EDGE('',*,*,#7322,.T.);
#9867=ORIENTED_EDGE('',*,*,#7318,.F.);
#9868=ORIENTED_EDGE('',*,*,#7323,.T.);
#9869=ORIENTED_EDGE('',*,*,#7324,.T.);
#9870=ORIENTED_EDGE('',*,*,#7325,.T.);
#9871=ORIENTED_EDGE('',*,*,#7321,.F.);
#9872=ORIENTED_EDGE('',*,*,#7326,.T.);
#9873=ORIENTED_EDGE('',*,*,#7327,.T.);
#9874=ORIENTED_EDGE('',*,*,#7328,.T.);
#9875=ORIENTED_EDGE('',*,*,#7324,.F.);
#9876=ORIENTED_EDGE('',*,*,#7329,.T.);
#9877=ORIENTED_EDGE('',*,*,#7313,.F.);
#9878=ORIENTED_EDGE('',*,*,#7330,.T.);
#9879=ORIENTED_EDGE('',*,*,#7327,.F.);
#9880=ORIENTED_EDGE('',*,*,#7293,.T.);
#9881=ORIENTED_EDGE('',*,*,#7282,.F.);
#9882=ORIENTED_EDGE('',*,*,#7331,.T.);
#9883=ORIENTED_EDGE('',*,*,#7320,.F.);
#9884=ORIENTED_EDGE('',*,*,#7297,.F.);
#9885=ORIENTED_EDGE('',*,*,#7312,.F.);
#9886=ORIENTED_EDGE('',*,*,#7315,.F.);
#9887=ORIENTED_EDGE('',*,*,#7317,.F.);
#9888=ORIENTED_EDGE('',*,*,#7319,.F.);
#9889=ORIENTED_EDGE('',*,*,#7322,.F.);
#9890=ORIENTED_EDGE('',*,*,#7325,.F.);
#9891=ORIENTED_EDGE('',*,*,#7328,.F.);
#9892=ORIENTED_EDGE('',*,*,#7330,.F.);
#9893=ORIENTED_EDGE('',*,*,#7332,.F.);
#9894=ORIENTED_EDGE('',*,*,#7333,.F.);
#9895=ORIENTED_EDGE('',*,*,#7334,.F.);
#9896=ORIENTED_EDGE('',*,*,#7335,.F.);
#9897=ORIENTED_EDGE('',*,*,#7336,.F.);
#9898=ORIENTED_EDGE('',*,*,#7337,.F.);
#9899=ORIENTED_EDGE('',*,*,#7338,.F.);
#9900=ORIENTED_EDGE('',*,*,#7339,.F.);
#9901=ORIENTED_EDGE('',*,*,#7340,.T.);
#9902=ORIENTED_EDGE('',*,*,#7332,.T.);
#9903=ORIENTED_EDGE('',*,*,#7341,.T.);
#9904=ORIENTED_EDGE('',*,*,#7159,.T.);
#9905=ORIENTED_EDGE('',*,*,#7342,.T.);
#9906=ORIENTED_EDGE('',*,*,#7333,.T.);
#9907=ORIENTED_EDGE('',*,*,#7340,.F.);
#9908=ORIENTED_EDGE('',*,*,#7227,.T.);
#9909=ORIENTED_EDGE('',*,*,#7343,.T.);
#9910=ORIENTED_EDGE('',*,*,#7334,.T.);
#9911=ORIENTED_EDGE('',*,*,#7342,.F.);
#9912=ORIENTED_EDGE('',*,*,#7193,.T.);
#9913=ORIENTED_EDGE('',*,*,#7344,.T.);
#9914=ORIENTED_EDGE('',*,*,#7335,.T.);
#9915=ORIENTED_EDGE('',*,*,#7343,.F.);
#9916=ORIENTED_EDGE('',*,*,#7345,.T.);
#9917=ORIENTED_EDGE('',*,*,#7346,.T.);
#9918=ORIENTED_EDGE('',*,*,#7336,.T.);
#9919=ORIENTED_EDGE('',*,*,#7344,.F.);
#9920=ORIENTED_EDGE('',*,*,#7347,.T.);
#9921=ORIENTED_EDGE('',*,*,#7348,.T.);
#9922=ORIENTED_EDGE('',*,*,#7337,.T.);
#9923=ORIENTED_EDGE('',*,*,#7346,.F.);
#9924=ORIENTED_EDGE('',*,*,#7349,.T.);
#9925=ORIENTED_EDGE('',*,*,#7350,.T.);
#9926=ORIENTED_EDGE('',*,*,#7338,.T.);
#9927=ORIENTED_EDGE('',*,*,#7348,.F.);
#9928=ORIENTED_EDGE('',*,*,#7351,.T.);
#9929=ORIENTED_EDGE('',*,*,#7341,.F.);
#9930=ORIENTED_EDGE('',*,*,#7339,.T.);
#9931=ORIENTED_EDGE('',*,*,#7350,.F.);
#9932=ORIENTED_EDGE('',*,*,#7225,.T.);
#9933=ORIENTED_EDGE('',*,*,#7207,.F.);
#9934=ORIENTED_EDGE('',*,*,#7352,.T.);
#9935=ORIENTED_EDGE('',*,*,#7345,.F.);
#9936=ORIENTED_EDGE('',*,*,#7192,.F.);
#9937=ORIENTED_EDGE('',*,*,#7216,.F.);
#9938=ORIENTED_EDGE('',*,*,#7226,.T.);
#9939=ORIENTED_EDGE('',*,*,#7351,.F.);
#9940=ORIENTED_EDGE('',*,*,#7353,.F.);
#9941=ORIENTED_EDGE('',*,*,#7213,.F.);
#9942=ORIENTED_EDGE('',*,*,#7353,.T.);
#9943=ORIENTED_EDGE('',*,*,#7349,.F.);
#9944=ORIENTED_EDGE('',*,*,#7354,.F.);
#9945=ORIENTED_EDGE('',*,*,#7210,.F.);
#9946=ORIENTED_EDGE('',*,*,#7354,.T.);
#9947=ORIENTED_EDGE('',*,*,#7347,.F.);
#9948=ORIENTED_EDGE('',*,*,#7352,.F.);
#9949=ORIENTED_EDGE('',*,*,#7288,.F.);
#9950=ORIENTED_EDGE('',*,*,#7294,.T.);
#9951=ORIENTED_EDGE('',*,*,#7329,.F.);
#9952=ORIENTED_EDGE('',*,*,#7355,.F.);
#9953=ORIENTED_EDGE('',*,*,#7286,.F.);
#9954=ORIENTED_EDGE('',*,*,#7355,.T.);
#9955=ORIENTED_EDGE('',*,*,#7326,.F.);
#9956=ORIENTED_EDGE('',*,*,#7356,.F.);
#9957=ORIENTED_EDGE('',*,*,#7284,.F.);
#9958=ORIENTED_EDGE('',*,*,#7356,.T.);
#9959=ORIENTED_EDGE('',*,*,#7323,.F.);
#9960=ORIENTED_EDGE('',*,*,#7331,.F.);
#9961=ORIENTED_EDGE('',*,*,#7357,.T.);
#9962=ORIENTED_EDGE('',*,*,#7358,.F.);
#9963=ORIENTED_EDGE('',*,*,#7359,.T.);
#9964=ORIENTED_EDGE('',*,*,#7360,.T.);
#9965=ORIENTED_EDGE('',*,*,#7361,.T.);
#9966=ORIENTED_EDGE('',*,*,#7362,.F.);
#9967=ORIENTED_EDGE('',*,*,#7363,.T.);
#9968=ORIENTED_EDGE('',*,*,#7364,.T.);
#9969=ORIENTED_EDGE('',*,*,#7362,.T.);
#9970=ORIENTED_EDGE('',*,*,#7365,.T.);
#9971=ORIENTED_EDGE('',*,*,#7366,.T.);
#9972=ORIENTED_EDGE('',*,*,#7367,.T.);
#9973=ORIENTED_EDGE('',*,*,#7368,.T.);
#9974=ORIENTED_EDGE('',*,*,#7369,.T.);
#9975=ORIENTED_EDGE('',*,*,#7370,.T.);
#9976=ORIENTED_EDGE('',*,*,#7371,.T.);
#9977=ORIENTED_EDGE('',*,*,#7370,.F.);
#9978=ORIENTED_EDGE('',*,*,#7372,.T.);
#9979=ORIENTED_EDGE('',*,*,#7366,.F.);
#9980=ORIENTED_EDGE('',*,*,#7373,.T.);
#9981=ORIENTED_EDGE('',*,*,#7358,.T.);
#9982=ORIENTED_EDGE('',*,*,#7374,.T.);
#9983=ORIENTED_EDGE('',*,*,#7375,.T.);
#9984=ORIENTED_EDGE('',*,*,#7376,.T.);
#9985=ORIENTED_EDGE('',*,*,#7375,.F.);
#9986=ORIENTED_EDGE('',*,*,#7377,.T.);
#9987=ORIENTED_EDGE('',*,*,#7368,.F.);
#9988=ORIENTED_EDGE('',*,*,#7378,.T.);
#9989=ORIENTED_EDGE('',*,*,#7374,.F.);
#9990=ORIENTED_EDGE('',*,*,#7357,.F.);
#9991=ORIENTED_EDGE('',*,*,#7379,.T.);
#9992=ORIENTED_EDGE('',*,*,#7380,.T.);
#9993=ORIENTED_EDGE('',*,*,#7381,.T.);
#9994=ORIENTED_EDGE('',*,*,#7360,.F.);
#9995=ORIENTED_EDGE('',*,*,#7382,.T.);
#9996=ORIENTED_EDGE('',*,*,#7383,.F.);
#9997=ORIENTED_EDGE('',*,*,#7384,.F.);
#9998=ORIENTED_EDGE('',*,*,#7385,.F.);
#9999=ORIENTED_EDGE('',*,*,#7379,.F.);
#10000=ORIENTED_EDGE('',*,*,#7359,.F.);
#10001=ORIENTED_EDGE('',*,*,#7376,.F.);
#10002=ORIENTED_EDGE('',*,*,#7378,.F.);
#10003=ORIENTED_EDGE('',*,*,#7371,.F.);
#10004=ORIENTED_EDGE('',*,*,#7373,.F.);
#10005=ORIENTED_EDGE('',*,*,#7365,.F.);
#10006=ORIENTED_EDGE('',*,*,#7361,.F.);
#10007=ORIENTED_EDGE('',*,*,#7386,.T.);
#10008=ORIENTED_EDGE('',*,*,#7387,.F.);
#10009=ORIENTED_EDGE('',*,*,#7388,.F.);
#10010=ORIENTED_EDGE('',*,*,#7389,.F.);
#10011=ORIENTED_EDGE('',*,*,#7390,.F.);
#10012=ORIENTED_EDGE('',*,*,#7391,.F.);
#10013=ORIENTED_EDGE('',*,*,#7392,.F.);
#10014=ORIENTED_EDGE('',*,*,#7393,.F.);
#10015=ORIENTED_EDGE('',*,*,#7382,.F.);
#10016=ORIENTED_EDGE('',*,*,#7394,.T.);
#10017=ORIENTED_EDGE('',*,*,#7395,.F.);
#10018=ORIENTED_EDGE('',*,*,#7396,.T.);
#10019=ORIENTED_EDGE('',*,*,#7397,.T.);
#10020=ORIENTED_EDGE('',*,*,#7398,.T.);
#10021=ORIENTED_EDGE('',*,*,#7399,.F.);
#10022=ORIENTED_EDGE('',*,*,#7400,.T.);
#10023=ORIENTED_EDGE('',*,*,#7401,.T.);
#10024=ORIENTED_EDGE('',*,*,#7399,.T.);
#10025=ORIENTED_EDGE('',*,*,#7402,.T.);
#10026=ORIENTED_EDGE('',*,*,#7403,.T.);
#10027=ORIENTED_EDGE('',*,*,#7404,.T.);
#10028=ORIENTED_EDGE('',*,*,#7405,.T.);
#10029=ORIENTED_EDGE('',*,*,#7406,.T.);
#10030=ORIENTED_EDGE('',*,*,#7407,.T.);
#10031=ORIENTED_EDGE('',*,*,#7408,.T.);
#10032=ORIENTED_EDGE('',*,*,#7407,.F.);
#10033=ORIENTED_EDGE('',*,*,#7409,.T.);
#10034=ORIENTED_EDGE('',*,*,#7403,.F.);
#10035=ORIENTED_EDGE('',*,*,#7410,.T.);
#10036=ORIENTED_EDGE('',*,*,#7395,.T.);
#10037=ORIENTED_EDGE('',*,*,#7411,.T.);
#10038=ORIENTED_EDGE('',*,*,#7412,.T.);
#10039=ORIENTED_EDGE('',*,*,#7413,.T.);
#10040=ORIENTED_EDGE('',*,*,#7412,.F.);
#10041=ORIENTED_EDGE('',*,*,#7414,.T.);
#10042=ORIENTED_EDGE('',*,*,#7405,.F.);
#10043=ORIENTED_EDGE('',*,*,#7415,.T.);
#10044=ORIENTED_EDGE('',*,*,#7401,.F.);
#10045=ORIENTED_EDGE('',*,*,#7416,.F.);
#10046=ORIENTED_EDGE('',*,*,#7417,.T.);
#10047=ORIENTED_EDGE('',*,*,#7418,.F.);
#10048=ORIENTED_EDGE('',*,*,#7419,.F.);
#10049=ORIENTED_EDGE('',*,*,#7420,.F.);
#10050=ORIENTED_EDGE('',*,*,#7400,.F.);
#10051=ORIENTED_EDGE('',*,*,#7404,.F.);
#10052=ORIENTED_EDGE('',*,*,#7421,.T.);
#10053=ORIENTED_EDGE('',*,*,#7422,.T.);
#10054=ORIENTED_EDGE('',*,*,#7416,.T.);
#10055=ORIENTED_EDGE('',*,*,#7377,.F.);
#10056=ORIENTED_EDGE('',*,*,#7381,.F.);
#10057=ORIENTED_EDGE('',*,*,#7423,.T.);
#10058=ORIENTED_EDGE('',*,*,#7424,.F.);
#10059=ORIENTED_EDGE('',*,*,#7425,.T.);
#10060=ORIENTED_EDGE('',*,*,#7421,.F.);
#10061=ORIENTED_EDGE('',*,*,#7409,.F.);
#10062=ORIENTED_EDGE('',*,*,#7406,.F.);
#10063=ORIENTED_EDGE('',*,*,#7414,.F.);
#10064=ORIENTED_EDGE('',*,*,#7426,.F.);
#10065=ORIENTED_EDGE('',*,*,#7372,.F.);
#10066=ORIENTED_EDGE('',*,*,#7369,.F.);
#10067=ORIENTED_EDGE('',*,*,#7427,.T.);
#10068=ORIENTED_EDGE('',*,*,#7428,.F.);
#10069=ORIENTED_EDGE('',*,*,#7387,.T.);
#10070=ORIENTED_EDGE('',*,*,#7429,.T.);
#10071=ORIENTED_EDGE('',*,*,#7393,.T.);
#10072=ORIENTED_EDGE('',*,*,#7430,.F.);
#10073=ORIENTED_EDGE('',*,*,#7431,.T.);
#10074=ORIENTED_EDGE('',*,*,#7383,.T.);
#10075=ORIENTED_EDGE('',*,*,#7430,.T.);
#10076=ORIENTED_EDGE('',*,*,#7392,.T.);
#10077=ORIENTED_EDGE('',*,*,#7432,.T.);
#10078=ORIENTED_EDGE('',*,*,#7433,.T.);
#10079=ORIENTED_EDGE('',*,*,#7434,.T.);
#10080=ORIENTED_EDGE('',*,*,#7435,.T.);
#10081=ORIENTED_EDGE('',*,*,#7436,.T.);
#10082=ORIENTED_EDGE('',*,*,#7390,.T.);
#10083=ORIENTED_EDGE('',*,*,#7436,.F.);
#10084=ORIENTED_EDGE('',*,*,#7437,.T.);
#10085=ORIENTED_EDGE('',*,*,#7432,.F.);
#10086=ORIENTED_EDGE('',*,*,#7391,.T.);
#10087=ORIENTED_EDGE('',*,*,#7428,.T.);
#10088=ORIENTED_EDGE('',*,*,#7438,.T.);
#10089=ORIENTED_EDGE('',*,*,#7439,.T.);
#10090=ORIENTED_EDGE('',*,*,#7388,.T.);
#10091=ORIENTED_EDGE('',*,*,#7439,.F.);
#10092=ORIENTED_EDGE('',*,*,#7440,.T.);
#10093=ORIENTED_EDGE('',*,*,#7434,.F.);
#10094=ORIENTED_EDGE('',*,*,#7389,.T.);
#10095=ORIENTED_EDGE('',*,*,#7438,.F.);
#10096=ORIENTED_EDGE('',*,*,#7427,.F.);
#10097=ORIENTED_EDGE('',*,*,#7441,.T.);
#10098=ORIENTED_EDGE('',*,*,#7442,.F.);
#10099=ORIENTED_EDGE('',*,*,#7443,.F.);
#10100=ORIENTED_EDGE('',*,*,#7444,.T.);
#10101=ORIENTED_EDGE('',*,*,#7364,.F.);
#10102=ORIENTED_EDGE('',*,*,#7445,.F.);
#10103=ORIENTED_EDGE('',*,*,#7397,.F.);
#10104=ORIENTED_EDGE('',*,*,#7446,.T.);
#10105=ORIENTED_EDGE('',*,*,#7447,.F.);
#10106=ORIENTED_EDGE('',*,*,#7441,.F.);
#10107=ORIENTED_EDGE('',*,*,#7429,.F.);
#10108=ORIENTED_EDGE('',*,*,#7386,.F.);
#10109=ORIENTED_EDGE('',*,*,#7448,.T.);
#10110=ORIENTED_EDGE('',*,*,#7449,.F.);
#10111=ORIENTED_EDGE('',*,*,#7450,.T.);
#10112=ORIENTED_EDGE('',*,*,#7419,.T.);
#10113=ORIENTED_EDGE('',*,*,#7451,.T.);
#10114=ORIENTED_EDGE('',*,*,#7452,.F.);
#10115=ORIENTED_EDGE('',*,*,#7442,.T.);
#10116=ORIENTED_EDGE('',*,*,#7447,.T.);
#10117=ORIENTED_EDGE('',*,*,#7452,.T.);
#10118=ORIENTED_EDGE('',*,*,#7453,.T.);
#10119=ORIENTED_EDGE('',*,*,#7454,.T.);
#10120=ORIENTED_EDGE('',*,*,#7443,.T.);
#10121=ORIENTED_EDGE('',*,*,#7455,.T.);
#10122=ORIENTED_EDGE('',*,*,#7456,.T.);
#10123=ORIENTED_EDGE('',*,*,#7457,.T.);
#10124=ORIENTED_EDGE('',*,*,#7458,.T.);
#10125=ORIENTED_EDGE('',*,*,#7457,.F.);
#10126=ORIENTED_EDGE('',*,*,#7459,.T.);
#10127=ORIENTED_EDGE('',*,*,#7454,.F.);
#10128=ORIENTED_EDGE('',*,*,#7460,.T.);
#10129=ORIENTED_EDGE('',*,*,#7449,.T.);
#10130=ORIENTED_EDGE('',*,*,#7461,.T.);
#10131=ORIENTED_EDGE('',*,*,#7462,.T.);
#10132=ORIENTED_EDGE('',*,*,#7463,.T.);
#10133=ORIENTED_EDGE('',*,*,#7462,.F.);
#10134=ORIENTED_EDGE('',*,*,#7464,.T.);
#10135=ORIENTED_EDGE('',*,*,#7455,.F.);
#10136=ORIENTED_EDGE('',*,*,#7465,.T.);
#10137=ORIENTED_EDGE('',*,*,#7440,.F.);
#10138=ORIENTED_EDGE('',*,*,#7444,.F.);
#10139=ORIENTED_EDGE('',*,*,#7459,.F.);
#10140=ORIENTED_EDGE('',*,*,#7456,.F.);
#10141=ORIENTED_EDGE('',*,*,#7464,.F.);
#10142=ORIENTED_EDGE('',*,*,#7466,.F.);
#10143=ORIENTED_EDGE('',*,*,#7467,.T.);
#10144=ORIENTED_EDGE('',*,*,#7468,.F.);
#10145=ORIENTED_EDGE('',*,*,#7469,.T.);
#10146=ORIENTED_EDGE('',*,*,#7470,.F.);
#10147=ORIENTED_EDGE('',*,*,#7437,.F.);
#10148=ORIENTED_EDGE('',*,*,#7435,.F.);
#10149=ORIENTED_EDGE('',*,*,#7398,.F.);
#10150=ORIENTED_EDGE('',*,*,#7420,.T.);
#10151=ORIENTED_EDGE('',*,*,#7450,.F.);
#10152=ORIENTED_EDGE('',*,*,#7463,.F.);
#10153=ORIENTED_EDGE('',*,*,#7465,.F.);
#10154=ORIENTED_EDGE('',*,*,#7458,.F.);
#10155=ORIENTED_EDGE('',*,*,#7460,.F.);
#10156=ORIENTED_EDGE('',*,*,#7453,.F.);
#10157=ORIENTED_EDGE('',*,*,#7451,.F.);
#10158=ORIENTED_EDGE('',*,*,#7446,.F.);
#10159=ORIENTED_EDGE('',*,*,#7396,.F.);
#10160=ORIENTED_EDGE('',*,*,#7413,.F.);
#10161=ORIENTED_EDGE('',*,*,#7415,.F.);
#10162=ORIENTED_EDGE('',*,*,#7408,.F.);
#10163=ORIENTED_EDGE('',*,*,#7410,.F.);
#10164=ORIENTED_EDGE('',*,*,#7402,.F.);
#10165=ORIENTED_EDGE('',*,*,#7367,.F.);
#10166=ORIENTED_EDGE('',*,*,#7426,.T.);
#10167=ORIENTED_EDGE('',*,*,#7411,.F.);
#10168=ORIENTED_EDGE('',*,*,#7394,.F.);
#10169=ORIENTED_EDGE('',*,*,#7445,.T.);
#10170=ORIENTED_EDGE('',*,*,#7363,.F.);
#10171=ORIENTED_EDGE('',*,*,#7448,.F.);
#10172=ORIENTED_EDGE('',*,*,#7418,.T.);
#10173=ORIENTED_EDGE('',*,*,#7471,.T.);
#10174=ORIENTED_EDGE('',*,*,#7466,.T.);
#10175=ORIENTED_EDGE('',*,*,#7461,.F.);
#10176=ORIENTED_EDGE('',*,*,#7471,.F.);
#10177=ORIENTED_EDGE('',*,*,#7417,.F.);
#10178=ORIENTED_EDGE('',*,*,#7422,.F.);
#10179=ORIENTED_EDGE('',*,*,#7425,.F.);
#10180=ORIENTED_EDGE('',*,*,#7472,.F.);
#10181=ORIENTED_EDGE('',*,*,#7473,.T.);
#10182=ORIENTED_EDGE('',*,*,#7474,.F.);
#10183=ORIENTED_EDGE('',*,*,#7467,.F.);
#10184=ORIENTED_EDGE('',*,*,#7475,.T.);
#10185=ORIENTED_EDGE('',*,*,#7468,.T.);
#10186=ORIENTED_EDGE('',*,*,#7474,.T.);
#10187=ORIENTED_EDGE('',*,*,#7476,.T.);
#10188=ORIENTED_EDGE('',*,*,#7475,.F.);
#10189=ORIENTED_EDGE('',*,*,#7477,.F.);
#10190=ORIENTED_EDGE('',*,*,#7478,.F.);
#10191=ORIENTED_EDGE('',*,*,#7423,.F.);
#10192=ORIENTED_EDGE('',*,*,#7380,.F.);
#10193=ORIENTED_EDGE('',*,*,#7385,.T.);
#10194=ORIENTED_EDGE('',*,*,#7479,.F.);
#10195=ORIENTED_EDGE('',*,*,#7469,.F.);
#10196=ORIENTED_EDGE('',*,*,#7476,.F.);
#10197=ORIENTED_EDGE('',*,*,#7473,.F.);
#10198=ORIENTED_EDGE('',*,*,#7480,.F.);
#10199=ORIENTED_EDGE('',*,*,#7477,.T.);
#10200=ORIENTED_EDGE('',*,*,#7472,.T.);
#10201=ORIENTED_EDGE('',*,*,#7424,.T.);
#10202=ORIENTED_EDGE('',*,*,#7478,.T.);
#10203=ORIENTED_EDGE('',*,*,#7480,.T.);
#10204=ORIENTED_EDGE('',*,*,#7433,.F.);
#10205=ORIENTED_EDGE('',*,*,#7470,.T.);
#10206=ORIENTED_EDGE('',*,*,#7479,.T.);
#10207=ORIENTED_EDGE('',*,*,#7384,.T.);
#10208=ORIENTED_EDGE('',*,*,#7431,.F.);
#10209=ORIENTED_EDGE('',*,*,#7481,.T.);
#10210=ORIENTED_EDGE('',*,*,#7482,.F.);
#10211=ORIENTED_EDGE('',*,*,#7483,.T.);
#10212=ORIENTED_EDGE('',*,*,#7484,.T.);
#10213=ORIENTED_EDGE('',*,*,#7485,.T.);
#10214=ORIENTED_EDGE('',*,*,#7486,.F.);
#10215=ORIENTED_EDGE('',*,*,#7487,.T.);
#10216=ORIENTED_EDGE('',*,*,#7488,.T.);
#10217=ORIENTED_EDGE('',*,*,#7486,.T.);
#10218=ORIENTED_EDGE('',*,*,#7489,.T.);
#10219=ORIENTED_EDGE('',*,*,#7490,.T.);
#10220=ORIENTED_EDGE('',*,*,#7491,.T.);
#10221=ORIENTED_EDGE('',*,*,#7490,.F.);
#10222=ORIENTED_EDGE('',*,*,#7492,.T.);
#10223=ORIENTED_EDGE('',*,*,#7493,.T.);
#10224=ORIENTED_EDGE('',*,*,#7494,.T.);
#10225=ORIENTED_EDGE('',*,*,#7482,.T.);
#10226=ORIENTED_EDGE('',*,*,#7495,.T.);
#10227=ORIENTED_EDGE('',*,*,#7493,.F.);
#10228=ORIENTED_EDGE('',*,*,#7496,.T.);
#10229=ORIENTED_EDGE('',*,*,#7484,.F.);
#10230=ORIENTED_EDGE('',*,*,#7497,.F.);
#10231=ORIENTED_EDGE('',*,*,#7498,.F.);
#10232=ORIENTED_EDGE('',*,*,#7499,.F.);
#10233=ORIENTED_EDGE('',*,*,#7500,.F.);
#10234=ORIENTED_EDGE('',*,*,#7501,.F.);
#10235=ORIENTED_EDGE('',*,*,#7502,.F.);
#10236=ORIENTED_EDGE('',*,*,#7503,.F.);
#10237=ORIENTED_EDGE('',*,*,#7483,.F.);
#10238=ORIENTED_EDGE('',*,*,#7496,.F.);
#10239=ORIENTED_EDGE('',*,*,#7504,.T.);
#10240=ORIENTED_EDGE('',*,*,#7505,.F.);
#10241=ORIENTED_EDGE('',*,*,#7506,.F.);
#10242=ORIENTED_EDGE('',*,*,#7497,.T.);
#10243=ORIENTED_EDGE('',*,*,#7492,.F.);
#10244=ORIENTED_EDGE('',*,*,#7507,.F.);
#10245=ORIENTED_EDGE('',*,*,#7508,.F.);
#10246=ORIENTED_EDGE('',*,*,#7504,.F.);
#10247=ORIENTED_EDGE('',*,*,#7489,.F.);
#10248=ORIENTED_EDGE('',*,*,#7485,.F.);
#10249=ORIENTED_EDGE('',*,*,#7509,.T.);
#10250=ORIENTED_EDGE('',*,*,#7510,.F.);
#10251=ORIENTED_EDGE('',*,*,#7511,.F.);
#10252=ORIENTED_EDGE('',*,*,#7507,.T.);
#10253=ORIENTED_EDGE('',*,*,#7512,.T.);
#10254=ORIENTED_EDGE('',*,*,#7513,.F.);
#10255=ORIENTED_EDGE('',*,*,#7510,.T.);
#10256=ORIENTED_EDGE('',*,*,#7514,.T.);
#10257=ORIENTED_EDGE('',*,*,#7506,.T.);
#10258=ORIENTED_EDGE('',*,*,#7515,.F.);
#10259=ORIENTED_EDGE('',*,*,#7516,.T.);
#10260=ORIENTED_EDGE('',*,*,#7498,.T.);
#10261=ORIENTED_EDGE('',*,*,#7515,.T.);
#10262=ORIENTED_EDGE('',*,*,#7505,.T.);
#10263=ORIENTED_EDGE('',*,*,#7517,.T.);
#10264=ORIENTED_EDGE('',*,*,#7518,.T.);
#10265=ORIENTED_EDGE('',*,*,#7519,.T.);
#10266=ORIENTED_EDGE('',*,*,#7520,.T.);
#10267=ORIENTED_EDGE('',*,*,#7517,.F.);
#10268=ORIENTED_EDGE('',*,*,#7508,.T.);
#10269=ORIENTED_EDGE('',*,*,#7513,.T.);
#10270=ORIENTED_EDGE('',*,*,#7521,.T.);
#10271=ORIENTED_EDGE('',*,*,#7519,.F.);
#10272=ORIENTED_EDGE('',*,*,#7511,.T.);
#10273=ORIENTED_EDGE('',*,*,#7522,.T.);
#10274=ORIENTED_EDGE('',*,*,#7523,.F.);
#10275=ORIENTED_EDGE('',*,*,#7524,.T.);
#10276=ORIENTED_EDGE('',*,*,#7500,.T.);
#10277=ORIENTED_EDGE('',*,*,#7525,.T.);
#10278=ORIENTED_EDGE('',*,*,#7526,.F.);
#10279=ORIENTED_EDGE('',*,*,#7527,.T.);
#10280=ORIENTED_EDGE('',*,*,#7528,.T.);
#10281=ORIENTED_EDGE('',*,*,#7526,.T.);
#10282=ORIENTED_EDGE('',*,*,#7529,.T.);
#10283=ORIENTED_EDGE('',*,*,#7530,.T.);
#10284=ORIENTED_EDGE('',*,*,#7531,.T.);
#10285=ORIENTED_EDGE('',*,*,#7530,.F.);
#10286=ORIENTED_EDGE('',*,*,#7532,.T.);
#10287=ORIENTED_EDGE('',*,*,#7533,.T.);
#10288=ORIENTED_EDGE('',*,*,#7534,.T.);
#10289=ORIENTED_EDGE('',*,*,#7523,.T.);
#10290=ORIENTED_EDGE('',*,*,#7535,.T.);
#10291=ORIENTED_EDGE('',*,*,#7533,.F.);
#10292=ORIENTED_EDGE('',*,*,#7536,.T.);
#10293=ORIENTED_EDGE('',*,*,#7524,.F.);
#10294=ORIENTED_EDGE('',*,*,#7536,.F.);
#10295=ORIENTED_EDGE('',*,*,#7537,.T.);
#10296=ORIENTED_EDGE('',*,*,#7538,.F.);
#10297=ORIENTED_EDGE('',*,*,#7539,.F.);
#10298=ORIENTED_EDGE('',*,*,#7501,.T.);
#10299=ORIENTED_EDGE('',*,*,#7532,.F.);
#10300=ORIENTED_EDGE('',*,*,#7540,.F.);
#10301=ORIENTED_EDGE('',*,*,#7541,.F.);
#10302=ORIENTED_EDGE('',*,*,#7537,.F.);
#10303=ORIENTED_EDGE('',*,*,#7529,.F.);
#10304=ORIENTED_EDGE('',*,*,#7525,.F.);
#10305=ORIENTED_EDGE('',*,*,#7542,.T.);
#10306=ORIENTED_EDGE('',*,*,#7543,.F.);
#10307=ORIENTED_EDGE('',*,*,#7544,.F.);
#10308=ORIENTED_EDGE('',*,*,#7540,.T.);
#10309=ORIENTED_EDGE('',*,*,#7488,.F.);
#10310=ORIENTED_EDGE('',*,*,#7545,.F.);
#10311=ORIENTED_EDGE('',*,*,#7546,.F.);
#10312=ORIENTED_EDGE('',*,*,#7542,.F.);
#10313=ORIENTED_EDGE('',*,*,#7528,.F.);
#10314=ORIENTED_EDGE('',*,*,#7547,.F.);
#10315=ORIENTED_EDGE('',*,*,#7514,.F.);
#10316=ORIENTED_EDGE('',*,*,#7509,.F.);
#10317=ORIENTED_EDGE('',*,*,#7539,.T.);
#10318=ORIENTED_EDGE('',*,*,#7548,.F.);
#10319=ORIENTED_EDGE('',*,*,#7549,.T.);
#10320=ORIENTED_EDGE('',*,*,#7502,.T.);
#10321=ORIENTED_EDGE('',*,*,#7550,.T.);
#10322=ORIENTED_EDGE('',*,*,#7551,.F.);
#10323=ORIENTED_EDGE('',*,*,#7543,.T.);
#10324=ORIENTED_EDGE('',*,*,#7546,.T.);
#10325=ORIENTED_EDGE('',*,*,#7551,.T.);
#10326=ORIENTED_EDGE('',*,*,#7552,.T.);
#10327=ORIENTED_EDGE('',*,*,#7553,.T.);
#10328=ORIENTED_EDGE('',*,*,#7544,.T.);
#10329=ORIENTED_EDGE('',*,*,#7553,.F.);
#10330=ORIENTED_EDGE('',*,*,#7554,.T.);
#10331=ORIENTED_EDGE('',*,*,#7555,.T.);
#10332=ORIENTED_EDGE('',*,*,#7541,.T.);
#10333=ORIENTED_EDGE('',*,*,#7548,.T.);
#10334=ORIENTED_EDGE('',*,*,#7538,.T.);
#10335=ORIENTED_EDGE('',*,*,#7555,.F.);
#10336=ORIENTED_EDGE('',*,*,#7556,.T.);
#10337=ORIENTED_EDGE('',*,*,#7481,.F.);
#10338=ORIENTED_EDGE('',*,*,#7503,.T.);
#10339=ORIENTED_EDGE('',*,*,#7549,.F.);
#10340=ORIENTED_EDGE('',*,*,#7556,.F.);
#10341=ORIENTED_EDGE('',*,*,#7557,.T.);
#10342=ORIENTED_EDGE('',*,*,#7495,.F.);
#10343=ORIENTED_EDGE('',*,*,#7494,.F.);
#10344=ORIENTED_EDGE('',*,*,#7557,.F.);
#10345=ORIENTED_EDGE('',*,*,#7554,.F.);
#10346=ORIENTED_EDGE('',*,*,#7558,.F.);
#10347=ORIENTED_EDGE('',*,*,#7491,.F.);
#10348=ORIENTED_EDGE('',*,*,#7558,.T.);
#10349=ORIENTED_EDGE('',*,*,#7552,.F.);
#10350=ORIENTED_EDGE('',*,*,#7550,.F.);
#10351=ORIENTED_EDGE('',*,*,#7545,.T.);
#10352=ORIENTED_EDGE('',*,*,#7487,.F.);
#10353=ORIENTED_EDGE('',*,*,#7512,.F.);
#10354=ORIENTED_EDGE('',*,*,#7547,.T.);
#10355=ORIENTED_EDGE('',*,*,#7527,.F.);
#10356=ORIENTED_EDGE('',*,*,#7531,.F.);
#10357=ORIENTED_EDGE('',*,*,#7559,.T.);
#10358=ORIENTED_EDGE('',*,*,#7521,.F.);
#10359=ORIENTED_EDGE('',*,*,#7520,.F.);
#10360=ORIENTED_EDGE('',*,*,#7559,.F.);
#10361=ORIENTED_EDGE('',*,*,#7534,.F.);
#10362=ORIENTED_EDGE('',*,*,#7560,.F.);
#10363=ORIENTED_EDGE('',*,*,#7518,.F.);
#10364=ORIENTED_EDGE('',*,*,#7560,.T.);
#10365=ORIENTED_EDGE('',*,*,#7535,.F.);
#10366=ORIENTED_EDGE('',*,*,#7522,.F.);
#10367=ORIENTED_EDGE('',*,*,#7499,.T.);
#10368=ORIENTED_EDGE('',*,*,#7516,.F.);
#10369=ORIENTED_EDGE('',*,*,#7561,.T.);
#10370=ORIENTED_EDGE('',*,*,#7562,.T.);
#10371=ORIENTED_EDGE('',*,*,#7563,.T.);
#10372=ORIENTED_EDGE('',*,*,#7564,.T.);
#10373=ORIENTED_EDGE('',*,*,#7563,.F.);
#10374=ORIENTED_EDGE('',*,*,#7565,.T.);
#10375=ORIENTED_EDGE('',*,*,#7566,.T.);
#10376=ORIENTED_EDGE('',*,*,#7567,.T.);
#10377=ORIENTED_EDGE('',*,*,#7568,.T.);
#10378=ORIENTED_EDGE('',*,*,#7569,.T.);
#10379=ORIENTED_EDGE('',*,*,#7566,.F.);
#10380=ORIENTED_EDGE('',*,*,#7570,.T.);
#10381=ORIENTED_EDGE('',*,*,#7571,.T.);
#10382=ORIENTED_EDGE('',*,*,#7570,.F.);
#10383=ORIENTED_EDGE('',*,*,#7572,.T.);
#10384=ORIENTED_EDGE('',*,*,#7573,.F.);
#10385=ORIENTED_EDGE('',*,*,#7574,.F.);
#10386=ORIENTED_EDGE('',*,*,#7575,.F.);
#10387=ORIENTED_EDGE('',*,*,#7576,.F.);
#10388=ORIENTED_EDGE('',*,*,#7565,.F.);
#10389=ORIENTED_EDGE('',*,*,#7577,.T.);
#10390=ORIENTED_EDGE('',*,*,#7578,.F.);
#10391=ORIENTED_EDGE('',*,*,#7572,.F.);
#10392=ORIENTED_EDGE('',*,*,#7579,.T.);
#10393=ORIENTED_EDGE('',*,*,#7562,.F.);
#10394=ORIENTED_EDGE('',*,*,#7580,.T.);
#10395=ORIENTED_EDGE('',*,*,#7581,.T.);
#10396=ORIENTED_EDGE('',*,*,#7582,.F.);
#10397=ORIENTED_EDGE('',*,*,#7583,.T.);
#10398=ORIENTED_EDGE('',*,*,#7584,.F.);
#10399=ORIENTED_EDGE('',*,*,#7577,.F.);
#10400=ORIENTED_EDGE('',*,*,#7585,.T.);
#10401=ORIENTED_EDGE('',*,*,#7586,.T.);
#10402=ORIENTED_EDGE('',*,*,#7587,.T.);
#10403=ORIENTED_EDGE('',*,*,#7586,.F.);
#10404=ORIENTED_EDGE('',*,*,#7588,.F.);
#10405=ORIENTED_EDGE('',*,*,#7589,.F.);
#10406=ORIENTED_EDGE('',*,*,#7590,.F.);
#10407=ORIENTED_EDGE('',*,*,#7591,.F.);
#10408=ORIENTED_EDGE('',*,*,#7592,.F.);
#10409=ORIENTED_EDGE('',*,*,#7593,.F.);
#10410=ORIENTED_EDGE('',*,*,#7594,.F.);
#10411=ORIENTED_EDGE('',*,*,#7595,.F.);
#10412=ORIENTED_EDGE('',*,*,#7585,.F.);
#10413=ORIENTED_EDGE('',*,*,#7587,.F.);
#10414=ORIENTED_EDGE('',*,*,#7596,.T.);
#10415=ORIENTED_EDGE('',*,*,#7597,.T.);
#10416=ORIENTED_EDGE('',*,*,#7596,.F.);
#10417=ORIENTED_EDGE('',*,*,#7598,.T.);
#10418=ORIENTED_EDGE('',*,*,#7599,.T.);
#10419=ORIENTED_EDGE('',*,*,#7600,.T.);
#10420=ORIENTED_EDGE('',*,*,#7601,.T.);
#10421=ORIENTED_EDGE('',*,*,#7600,.F.);
#10422=ORIENTED_EDGE('',*,*,#7602,.T.);
#10423=ORIENTED_EDGE('',*,*,#7603,.T.);
#10424=ORIENTED_EDGE('',*,*,#7604,.T.);
#10425=ORIENTED_EDGE('',*,*,#7605,.T.);
#10426=ORIENTED_EDGE('',*,*,#7606,.T.);
#10427=ORIENTED_EDGE('',*,*,#7603,.F.);
#10428=ORIENTED_EDGE('',*,*,#7607,.T.);
#10429=ORIENTED_EDGE('',*,*,#7608,.T.);
#10430=ORIENTED_EDGE('',*,*,#7607,.F.);
#10431=ORIENTED_EDGE('',*,*,#7609,.T.);
#10432=ORIENTED_EDGE('',*,*,#7610,.F.);
#10433=ORIENTED_EDGE('',*,*,#7611,.F.);
#10434=ORIENTED_EDGE('',*,*,#7612,.F.);
#10435=ORIENTED_EDGE('',*,*,#7613,.F.);
#10436=ORIENTED_EDGE('',*,*,#7602,.F.);
#10437=ORIENTED_EDGE('',*,*,#7614,.T.);
#10438=ORIENTED_EDGE('',*,*,#7615,.F.);
#10439=ORIENTED_EDGE('',*,*,#7609,.F.);
#10440=ORIENTED_EDGE('',*,*,#7616,.T.);
#10441=ORIENTED_EDGE('',*,*,#7599,.F.);
#10442=ORIENTED_EDGE('',*,*,#7617,.T.);
#10443=ORIENTED_EDGE('',*,*,#7618,.T.);
#10444=ORIENTED_EDGE('',*,*,#7619,.F.);
#10445=ORIENTED_EDGE('',*,*,#7620,.T.);
#10446=ORIENTED_EDGE('',*,*,#7621,.F.);
#10447=ORIENTED_EDGE('',*,*,#7614,.F.);
#10448=ORIENTED_EDGE('',*,*,#7618,.F.);
#10449=ORIENTED_EDGE('',*,*,#7622,.T.);
#10450=ORIENTED_EDGE('',*,*,#7623,.T.);
#10451=ORIENTED_EDGE('',*,*,#7624,.T.);
#10452=ORIENTED_EDGE('',*,*,#7625,.T.);
#10453=ORIENTED_EDGE('',*,*,#7626,.T.);
#10454=ORIENTED_EDGE('',*,*,#7623,.F.);
#10455=ORIENTED_EDGE('',*,*,#7627,.T.);
#10456=ORIENTED_EDGE('',*,*,#7628,.T.);
#10457=ORIENTED_EDGE('',*,*,#7629,.T.);
#10458=ORIENTED_EDGE('',*,*,#7625,.F.);
#10459=ORIENTED_EDGE('',*,*,#7630,.T.);
#10460=ORIENTED_EDGE('',*,*,#7631,.T.);
#10461=ORIENTED_EDGE('',*,*,#7632,.T.);
#10462=ORIENTED_EDGE('',*,*,#7628,.F.);
#10463=ORIENTED_EDGE('',*,*,#7633,.T.);
#10464=ORIENTED_EDGE('',*,*,#7576,.T.);
#10465=ORIENTED_EDGE('',*,*,#7634,.T.);
#10466=ORIENTED_EDGE('',*,*,#7631,.F.);
#10467=ORIENTED_EDGE('',*,*,#7635,.T.);
#10468=ORIENTED_EDGE('',*,*,#7571,.F.);
#10469=ORIENTED_EDGE('',*,*,#7635,.F.);
#10470=ORIENTED_EDGE('',*,*,#7636,.F.);
#10471=ORIENTED_EDGE('',*,*,#7637,.F.);
#10472=ORIENTED_EDGE('',*,*,#7638,.T.);
#10473=ORIENTED_EDGE('',*,*,#7639,.F.);
#10474=ORIENTED_EDGE('',*,*,#7640,.F.);
#10475=ORIENTED_EDGE('',*,*,#7641,.F.);
#10476=ORIENTED_EDGE('',*,*,#7642,.T.);
#10477=ORIENTED_EDGE('',*,*,#7643,.F.);
#10478=ORIENTED_EDGE('',*,*,#7580,.F.);
#10479=ORIENTED_EDGE('',*,*,#7561,.F.);
#10480=ORIENTED_EDGE('',*,*,#7644,.F.);
#10481=ORIENTED_EDGE('',*,*,#7568,.F.);
#10482=ORIENTED_EDGE('',*,*,#7633,.F.);
#10483=ORIENTED_EDGE('',*,*,#7645,.F.);
#10484=ORIENTED_EDGE('',*,*,#7646,.F.);
#10485=ORIENTED_EDGE('',*,*,#7636,.T.);
#10486=ORIENTED_EDGE('',*,*,#7630,.F.);
#10487=ORIENTED_EDGE('',*,*,#7647,.F.);
#10488=ORIENTED_EDGE('',*,*,#7648,.F.);
#10489=ORIENTED_EDGE('',*,*,#7645,.T.);
#10490=ORIENTED_EDGE('',*,*,#7627,.F.);
#10491=ORIENTED_EDGE('',*,*,#7649,.F.);
#10492=ORIENTED_EDGE('',*,*,#7650,.F.);
#10493=ORIENTED_EDGE('',*,*,#7647,.T.);
#10494=ORIENTED_EDGE('',*,*,#7622,.F.);
#10495=ORIENTED_EDGE('',*,*,#7617,.F.);
#10496=ORIENTED_EDGE('',*,*,#7598,.F.);
#10497=ORIENTED_EDGE('',*,*,#7651,.F.);
#10498=ORIENTED_EDGE('',*,*,#7605,.F.);
#10499=ORIENTED_EDGE('',*,*,#7608,.F.);
#10500=ORIENTED_EDGE('',*,*,#7652,.F.);
#10501=ORIENTED_EDGE('',*,*,#7653,.F.);
#10502=ORIENTED_EDGE('',*,*,#7654,.F.);
#10503=ORIENTED_EDGE('',*,*,#7655,.F.);
#10504=ORIENTED_EDGE('',*,*,#7656,.F.);
#10505=ORIENTED_EDGE('',*,*,#7657,.F.);
#10506=ORIENTED_EDGE('',*,*,#7658,.F.);
#10507=ORIENTED_EDGE('',*,*,#7649,.T.);
#10508=ORIENTED_EDGE('',*,*,#7581,.F.);
#10509=ORIENTED_EDGE('',*,*,#7643,.T.);
#10510=ORIENTED_EDGE('',*,*,#7659,.T.);
#10511=ORIENTED_EDGE('',*,*,#7660,.T.);
#10512=ORIENTED_EDGE('',*,*,#7661,.T.);
#10513=ORIENTED_EDGE('',*,*,#7662,.T.);
#10514=ORIENTED_EDGE('',*,*,#7659,.F.);
#10515=ORIENTED_EDGE('',*,*,#7663,.T.);
#10516=ORIENTED_EDGE('',*,*,#7664,.T.);
#10517=ORIENTED_EDGE('',*,*,#7665,.T.);
#10518=ORIENTED_EDGE('',*,*,#7661,.F.);
#10519=ORIENTED_EDGE('',*,*,#7666,.T.);
#10520=ORIENTED_EDGE('',*,*,#7667,.T.);
#10521=ORIENTED_EDGE('',*,*,#7668,.T.);
#10522=ORIENTED_EDGE('',*,*,#7664,.F.);
#10523=ORIENTED_EDGE('',*,*,#7669,.T.);
#10524=ORIENTED_EDGE('',*,*,#7613,.T.);
#10525=ORIENTED_EDGE('',*,*,#7670,.T.);
#10526=ORIENTED_EDGE('',*,*,#7667,.F.);
#10527=ORIENTED_EDGE('',*,*,#7652,.T.);
#10528=ORIENTED_EDGE('',*,*,#7669,.F.);
#10529=ORIENTED_EDGE('',*,*,#7671,.F.);
#10530=ORIENTED_EDGE('',*,*,#7672,.F.);
#10531=ORIENTED_EDGE('',*,*,#7653,.T.);
#10532=ORIENTED_EDGE('',*,*,#7666,.F.);
#10533=ORIENTED_EDGE('',*,*,#7673,.F.);
#10534=ORIENTED_EDGE('',*,*,#7674,.F.);
#10535=ORIENTED_EDGE('',*,*,#7671,.T.);
#10536=ORIENTED_EDGE('',*,*,#7663,.F.);
#10537=ORIENTED_EDGE('',*,*,#7642,.F.);
#10538=ORIENTED_EDGE('',*,*,#7675,.F.);
#10539=ORIENTED_EDGE('',*,*,#7673,.T.);
#10540=ORIENTED_EDGE('',*,*,#7676,.T.);
#10541=ORIENTED_EDGE('',*,*,#7588,.T.);
#10542=ORIENTED_EDGE('',*,*,#7677,.T.);
#10543=ORIENTED_EDGE('',*,*,#7678,.T.);
#10544=ORIENTED_EDGE('',*,*,#7676,.F.);
#10545=ORIENTED_EDGE('',*,*,#7637,.T.);
#10546=ORIENTED_EDGE('',*,*,#7679,.T.);
#10547=ORIENTED_EDGE('',*,*,#7589,.T.);
#10548=ORIENTED_EDGE('',*,*,#7680,.T.);
#10549=ORIENTED_EDGE('',*,*,#7590,.T.);
#10550=ORIENTED_EDGE('',*,*,#7679,.F.);
#10551=ORIENTED_EDGE('',*,*,#7646,.T.);
#10552=ORIENTED_EDGE('',*,*,#7680,.F.);
#10553=ORIENTED_EDGE('',*,*,#7648,.T.);
#10554=ORIENTED_EDGE('',*,*,#7681,.T.);
#10555=ORIENTED_EDGE('',*,*,#7591,.T.);
#10556=ORIENTED_EDGE('',*,*,#7682,.T.);
#10557=ORIENTED_EDGE('',*,*,#7592,.T.);
#10558=ORIENTED_EDGE('',*,*,#7681,.F.);
#10559=ORIENTED_EDGE('',*,*,#7650,.T.);
#10560=ORIENTED_EDGE('',*,*,#7682,.F.);
#10561=ORIENTED_EDGE('',*,*,#7658,.T.);
#10562=ORIENTED_EDGE('',*,*,#7683,.T.);
#10563=ORIENTED_EDGE('',*,*,#7593,.T.);
#10564=ORIENTED_EDGE('',*,*,#7684,.T.);
#10565=ORIENTED_EDGE('',*,*,#7594,.T.);
#10566=ORIENTED_EDGE('',*,*,#7683,.F.);
#10567=ORIENTED_EDGE('',*,*,#7685,.T.);
#10568=ORIENTED_EDGE('',*,*,#7684,.F.);
#10569=ORIENTED_EDGE('',*,*,#7686,.T.);
#10570=ORIENTED_EDGE('',*,*,#7677,.F.);
#10571=ORIENTED_EDGE('',*,*,#7595,.T.);
#10572=ORIENTED_EDGE('',*,*,#7678,.F.);
#10573=ORIENTED_EDGE('',*,*,#7687,.T.);
#10574=ORIENTED_EDGE('',*,*,#7688,.F.);
#10575=ORIENTED_EDGE('',*,*,#7638,.F.);
#10576=ORIENTED_EDGE('',*,*,#7689,.T.);
#10577=ORIENTED_EDGE('',*,*,#7690,.T.);
#10578=ORIENTED_EDGE('',*,*,#7691,.T.);
#10579=ORIENTED_EDGE('',*,*,#7655,.T.);
#10580=ORIENTED_EDGE('',*,*,#7690,.F.);
#10581=ORIENTED_EDGE('',*,*,#7692,.F.);
#10582=ORIENTED_EDGE('',*,*,#7693,.F.);
#10583=ORIENTED_EDGE('',*,*,#7694,.F.);
#10584=ORIENTED_EDGE('',*,*,#7695,.T.);
#10585=ORIENTED_EDGE('',*,*,#7693,.T.);
#10586=ORIENTED_EDGE('',*,*,#7696,.T.);
#10587=ORIENTED_EDGE('',*,*,#7640,.T.);
#10588=ORIENTED_EDGE('',*,*,#7697,.T.);
#10589=ORIENTED_EDGE('',*,*,#7698,.T.);
#10590=ORIENTED_EDGE('',*,*,#7699,.T.);
#10591=ORIENTED_EDGE('',*,*,#7573,.T.);
#10592=ORIENTED_EDGE('',*,*,#7700,.T.);
#10593=ORIENTED_EDGE('',*,*,#7701,.T.);
#10594=ORIENTED_EDGE('',*,*,#7697,.F.);
#10595=ORIENTED_EDGE('',*,*,#7578,.T.);
#10596=ORIENTED_EDGE('',*,*,#7702,.T.);
#10597=ORIENTED_EDGE('',*,*,#7703,.T.);
#10598=ORIENTED_EDGE('',*,*,#7700,.F.);
#10599=ORIENTED_EDGE('',*,*,#7584,.T.);
#10600=ORIENTED_EDGE('',*,*,#7704,.T.);
#10601=ORIENTED_EDGE('',*,*,#7705,.T.);
#10602=ORIENTED_EDGE('',*,*,#7702,.F.);
#10603=ORIENTED_EDGE('',*,*,#7706,.T.);
#10604=ORIENTED_EDGE('',*,*,#7707,.T.);
#10605=ORIENTED_EDGE('',*,*,#7708,.T.);
#10606=ORIENTED_EDGE('',*,*,#7704,.F.);
#10607=ORIENTED_EDGE('',*,*,#7610,.T.);
#10608=ORIENTED_EDGE('',*,*,#7709,.T.);
#10609=ORIENTED_EDGE('',*,*,#7710,.T.);
#10610=ORIENTED_EDGE('',*,*,#7707,.F.);
#10611=ORIENTED_EDGE('',*,*,#7615,.T.);
#10612=ORIENTED_EDGE('',*,*,#7711,.T.);
#10613=ORIENTED_EDGE('',*,*,#7712,.T.);
#10614=ORIENTED_EDGE('',*,*,#7709,.F.);
#10615=ORIENTED_EDGE('',*,*,#7621,.T.);
#10616=ORIENTED_EDGE('',*,*,#7699,.F.);
#10617=ORIENTED_EDGE('',*,*,#7713,.T.);
#10618=ORIENTED_EDGE('',*,*,#7711,.F.);
#10619=ORIENTED_EDGE('',*,*,#7714,.T.);
#10620=ORIENTED_EDGE('',*,*,#7706,.F.);
#10621=ORIENTED_EDGE('',*,*,#7583,.F.);
#10622=ORIENTED_EDGE('',*,*,#7715,.F.);
#10623=ORIENTED_EDGE('',*,*,#7611,.T.);
#10624=ORIENTED_EDGE('',*,*,#7698,.F.);
#10625=ORIENTED_EDGE('',*,*,#7701,.F.);
#10626=ORIENTED_EDGE('',*,*,#7703,.F.);
#10627=ORIENTED_EDGE('',*,*,#7705,.F.);
#10628=ORIENTED_EDGE('',*,*,#7708,.F.);
#10629=ORIENTED_EDGE('',*,*,#7710,.F.);
#10630=ORIENTED_EDGE('',*,*,#7712,.F.);
#10631=ORIENTED_EDGE('',*,*,#7713,.F.);
#10632=ORIENTED_EDGE('',*,*,#7716,.F.);
#10633=ORIENTED_EDGE('',*,*,#7717,.F.);
#10634=ORIENTED_EDGE('',*,*,#7718,.F.);
#10635=ORIENTED_EDGE('',*,*,#7719,.F.);
#10636=ORIENTED_EDGE('',*,*,#7720,.F.);
#10637=ORIENTED_EDGE('',*,*,#7721,.F.);
#10638=ORIENTED_EDGE('',*,*,#7722,.F.);
#10639=ORIENTED_EDGE('',*,*,#7723,.F.);
#10640=ORIENTED_EDGE('',*,*,#7724,.F.);
#10641=ORIENTED_EDGE('',*,*,#7725,.F.);
#10642=ORIENTED_EDGE('',*,*,#7726,.F.);
#10643=ORIENTED_EDGE('',*,*,#7727,.F.);
#10644=ORIENTED_EDGE('',*,*,#7728,.F.);
#10645=ORIENTED_EDGE('',*,*,#7729,.F.);
#10646=ORIENTED_EDGE('',*,*,#7730,.F.);
#10647=ORIENTED_EDGE('',*,*,#7731,.F.);
#10648=ORIENTED_EDGE('',*,*,#7732,.T.);
#10649=ORIENTED_EDGE('',*,*,#7733,.T.);
#10650=ORIENTED_EDGE('',*,*,#7656,.T.);
#10651=ORIENTED_EDGE('',*,*,#7691,.F.);
#10652=ORIENTED_EDGE('',*,*,#7734,.T.);
#10653=ORIENTED_EDGE('',*,*,#7735,.T.);
#10654=ORIENTED_EDGE('',*,*,#7733,.F.);
#10655=ORIENTED_EDGE('',*,*,#7736,.T.);
#10656=ORIENTED_EDGE('',*,*,#7737,.T.);
#10657=ORIENTED_EDGE('',*,*,#7738,.T.);
#10658=ORIENTED_EDGE('',*,*,#7734,.F.);
#10659=ORIENTED_EDGE('',*,*,#7739,.T.);
#10660=ORIENTED_EDGE('',*,*,#7740,.T.);
#10661=ORIENTED_EDGE('',*,*,#7688,.T.);
#10662=ORIENTED_EDGE('',*,*,#7737,.F.);
#10663=ORIENTED_EDGE('',*,*,#7741,.T.);
#10664=ORIENTED_EDGE('',*,*,#7639,.T.);
#10665=ORIENTED_EDGE('',*,*,#7740,.F.);
#10666=ORIENTED_EDGE('',*,*,#7742,.T.);
#10667=ORIENTED_EDGE('',*,*,#7695,.F.);
#10668=ORIENTED_EDGE('',*,*,#7742,.F.);
#10669=ORIENTED_EDGE('',*,*,#7741,.F.);
#10670=ORIENTED_EDGE('',*,*,#7739,.F.);
#10671=ORIENTED_EDGE('',*,*,#7736,.F.);
#10672=ORIENTED_EDGE('',*,*,#7732,.F.);
#10673=ORIENTED_EDGE('',*,*,#7694,.T.);
#10674=ORIENTED_EDGE('',*,*,#7743,.T.);
#10675=ORIENTED_EDGE('',*,*,#7744,.T.);
#10676=ORIENTED_EDGE('',*,*,#7641,.T.);
#10677=ORIENTED_EDGE('',*,*,#7696,.F.);
#10678=ORIENTED_EDGE('',*,*,#7745,.T.);
#10679=ORIENTED_EDGE('',*,*,#7675,.T.);
#10680=ORIENTED_EDGE('',*,*,#7744,.F.);
#10681=ORIENTED_EDGE('',*,*,#7746,.T.);
#10682=ORIENTED_EDGE('',*,*,#7747,.T.);
#10683=ORIENTED_EDGE('',*,*,#7674,.T.);
#10684=ORIENTED_EDGE('',*,*,#7745,.F.);
#10685=ORIENTED_EDGE('',*,*,#7748,.T.);
#10686=ORIENTED_EDGE('',*,*,#7749,.T.);
#10687=ORIENTED_EDGE('',*,*,#7672,.T.);
#10688=ORIENTED_EDGE('',*,*,#7747,.F.);
#10689=ORIENTED_EDGE('',*,*,#7750,.T.);
#10690=ORIENTED_EDGE('',*,*,#7654,.T.);
#10691=ORIENTED_EDGE('',*,*,#7749,.F.);
#10692=ORIENTED_EDGE('',*,*,#7751,.T.);
#10693=ORIENTED_EDGE('',*,*,#7689,.F.);
#10694=ORIENTED_EDGE('',*,*,#7751,.F.);
#10695=ORIENTED_EDGE('',*,*,#7750,.F.);
#10696=ORIENTED_EDGE('',*,*,#7748,.F.);
#10697=ORIENTED_EDGE('',*,*,#7746,.F.);
#10698=ORIENTED_EDGE('',*,*,#7743,.F.);
#10699=ORIENTED_EDGE('',*,*,#7692,.T.);
#10700=ORIENTED_EDGE('',*,*,#7718,.T.);
#10701=ORIENTED_EDGE('',*,*,#7752,.T.);
#10702=ORIENTED_EDGE('',*,*,#7753,.T.);
#10703=ORIENTED_EDGE('',*,*,#7754,.F.);
#10704=ORIENTED_EDGE('',*,*,#7716,.T.);
#10705=ORIENTED_EDGE('',*,*,#7755,.T.);
#10706=ORIENTED_EDGE('',*,*,#7756,.T.);
#10707=ORIENTED_EDGE('',*,*,#7757,.T.);
#10708=ORIENTED_EDGE('',*,*,#7758,.T.);
#10709=ORIENTED_EDGE('',*,*,#7755,.F.);
#10710=ORIENTED_EDGE('',*,*,#7719,.T.);
#10711=ORIENTED_EDGE('',*,*,#7754,.T.);
#10712=ORIENTED_EDGE('',*,*,#7717,.T.);
#10713=ORIENTED_EDGE('',*,*,#7757,.F.);
#10714=ORIENTED_EDGE('',*,*,#7759,.T.);
#10715=ORIENTED_EDGE('',*,*,#7752,.F.);
#10716=ORIENTED_EDGE('',*,*,#7759,.F.);
#10717=ORIENTED_EDGE('',*,*,#7760,.T.);
#10718=ORIENTED_EDGE('',*,*,#7761,.T.);
#10719=ORIENTED_EDGE('',*,*,#7762,.F.);
#10720=ORIENTED_EDGE('',*,*,#7756,.F.);
#10721=ORIENTED_EDGE('',*,*,#7763,.T.);
#10722=ORIENTED_EDGE('',*,*,#7764,.T.);
#10723=ORIENTED_EDGE('',*,*,#7760,.F.);
#10724=ORIENTED_EDGE('',*,*,#7765,.T.);
#10725=ORIENTED_EDGE('',*,*,#7730,.T.);
#10726=ORIENTED_EDGE('',*,*,#7766,.T.);
#10727=ORIENTED_EDGE('',*,*,#7767,.T.);
#10728=ORIENTED_EDGE('',*,*,#7768,.F.);
#10729=ORIENTED_EDGE('',*,*,#7728,.T.);
#10730=ORIENTED_EDGE('',*,*,#7769,.T.);
#10731=ORIENTED_EDGE('',*,*,#7770,.T.);
#10732=ORIENTED_EDGE('',*,*,#7771,.T.);
#10733=ORIENTED_EDGE('',*,*,#7772,.T.);
#10734=ORIENTED_EDGE('',*,*,#7769,.F.);
#10735=ORIENTED_EDGE('',*,*,#7731,.T.);
#10736=ORIENTED_EDGE('',*,*,#7768,.T.);
#10737=ORIENTED_EDGE('',*,*,#7729,.T.);
#10738=ORIENTED_EDGE('',*,*,#7771,.F.);
#10739=ORIENTED_EDGE('',*,*,#7773,.T.);
#10740=ORIENTED_EDGE('',*,*,#7766,.F.);
#10741=ORIENTED_EDGE('',*,*,#7773,.F.);
#10742=ORIENTED_EDGE('',*,*,#7774,.T.);
#10743=ORIENTED_EDGE('',*,*,#7775,.T.);
#10744=ORIENTED_EDGE('',*,*,#7776,.F.);
#10745=ORIENTED_EDGE('',*,*,#7770,.F.);
#10746=ORIENTED_EDGE('',*,*,#7777,.T.);
#10747=ORIENTED_EDGE('',*,*,#7778,.T.);
#10748=ORIENTED_EDGE('',*,*,#7774,.F.);
#10749=ORIENTED_EDGE('',*,*,#7779,.T.);
#10750=ORIENTED_EDGE('',*,*,#7722,.T.);
#10751=ORIENTED_EDGE('',*,*,#7780,.T.);
#10752=ORIENTED_EDGE('',*,*,#7781,.T.);
#10753=ORIENTED_EDGE('',*,*,#7782,.F.);
#10754=ORIENTED_EDGE('',*,*,#7720,.T.);
#10755=ORIENTED_EDGE('',*,*,#7783,.T.);
#10756=ORIENTED_EDGE('',*,*,#7784,.T.);
#10757=ORIENTED_EDGE('',*,*,#7785,.T.);
#10758=ORIENTED_EDGE('',*,*,#7786,.T.);
#10759=ORIENTED_EDGE('',*,*,#7783,.F.);
#10760=ORIENTED_EDGE('',*,*,#7723,.T.);
#10761=ORIENTED_EDGE('',*,*,#7782,.T.);
#10762=ORIENTED_EDGE('',*,*,#7721,.T.);
#10763=ORIENTED_EDGE('',*,*,#7785,.F.);
#10764=ORIENTED_EDGE('',*,*,#7787,.T.);
#10765=ORIENTED_EDGE('',*,*,#7780,.F.);
#10766=ORIENTED_EDGE('',*,*,#7787,.F.);
#10767=ORIENTED_EDGE('',*,*,#7788,.T.);
#10768=ORIENTED_EDGE('',*,*,#7789,.T.);
#10769=ORIENTED_EDGE('',*,*,#7790,.F.);
#10770=ORIENTED_EDGE('',*,*,#7784,.F.);
#10771=ORIENTED_EDGE('',*,*,#7791,.T.);
#10772=ORIENTED_EDGE('',*,*,#7792,.T.);
#10773=ORIENTED_EDGE('',*,*,#7788,.F.);
#10774=ORIENTED_EDGE('',*,*,#7793,.T.);
#10775=ORIENTED_EDGE('',*,*,#7726,.T.);
#10776=ORIENTED_EDGE('',*,*,#7794,.T.);
#10777=ORIENTED_EDGE('',*,*,#7795,.T.);
#10778=ORIENTED_EDGE('',*,*,#7796,.F.);
#10779=ORIENTED_EDGE('',*,*,#7724,.T.);
#10780=ORIENTED_EDGE('',*,*,#7797,.T.);
#10781=ORIENTED_EDGE('',*,*,#7798,.T.);
#10782=ORIENTED_EDGE('',*,*,#7799,.T.);
#10783=ORIENTED_EDGE('',*,*,#7800,.T.);
#10784=ORIENTED_EDGE('',*,*,#7797,.F.);
#10785=ORIENTED_EDGE('',*,*,#7727,.T.);
#10786=ORIENTED_EDGE('',*,*,#7796,.T.);
#10787=ORIENTED_EDGE('',*,*,#7725,.T.);
#10788=ORIENTED_EDGE('',*,*,#7799,.F.);
#10789=ORIENTED_EDGE('',*,*,#7801,.T.);
#10790=ORIENTED_EDGE('',*,*,#7794,.F.);
#10791=ORIENTED_EDGE('',*,*,#7801,.F.);
#10792=ORIENTED_EDGE('',*,*,#7802,.T.);
#10793=ORIENTED_EDGE('',*,*,#7803,.T.);
#10794=ORIENTED_EDGE('',*,*,#7804,.F.);
#10795=ORIENTED_EDGE('',*,*,#7798,.F.);
#10796=ORIENTED_EDGE('',*,*,#7805,.T.);
#10797=ORIENTED_EDGE('',*,*,#7806,.T.);
#10798=ORIENTED_EDGE('',*,*,#7802,.F.);
#10799=ORIENTED_EDGE('',*,*,#7807,.T.);
#10800=ORIENTED_EDGE('',*,*,#7579,.F.);
#10801=ORIENTED_EDGE('',*,*,#7808,.T.);
#10802=ORIENTED_EDGE('',*,*,#7809,.F.);
#10803=ORIENTED_EDGE('',*,*,#7808,.F.);
#10804=ORIENTED_EDGE('',*,*,#7793,.F.);
#10805=ORIENTED_EDGE('',*,*,#7810,.T.);
#10806=ORIENTED_EDGE('',*,*,#7811,.F.);
#10807=ORIENTED_EDGE('',*,*,#7810,.F.);
#10808=ORIENTED_EDGE('',*,*,#7807,.F.);
#10809=ORIENTED_EDGE('',*,*,#7812,.T.);
#10810=ORIENTED_EDGE('',*,*,#7813,.F.);
#10811=ORIENTED_EDGE('',*,*,#7812,.F.);
#10812=ORIENTED_EDGE('',*,*,#7765,.F.);
#10813=ORIENTED_EDGE('',*,*,#7814,.T.);
#10814=ORIENTED_EDGE('',*,*,#7815,.F.);
#10815=ORIENTED_EDGE('',*,*,#7814,.F.);
#10816=ORIENTED_EDGE('',*,*,#7779,.F.);
#10817=ORIENTED_EDGE('',*,*,#7816,.T.);
#10818=ORIENTED_EDGE('',*,*,#7616,.F.);
#10819=ORIENTED_EDGE('',*,*,#7816,.F.);
#10820=ORIENTED_EDGE('',*,*,#7800,.F.);
#10821=ORIENTED_EDGE('',*,*,#7817,.T.);
#10822=ORIENTED_EDGE('',*,*,#7818,.T.);
#10823=ORIENTED_EDGE('',*,*,#7805,.F.);
#10824=ORIENTED_EDGE('',*,*,#7795,.F.);
#10825=ORIENTED_EDGE('',*,*,#7804,.T.);
#10826=ORIENTED_EDGE('',*,*,#7819,.T.);
#10827=ORIENTED_EDGE('',*,*,#7817,.F.);
#10828=ORIENTED_EDGE('',*,*,#7815,.T.);
#10829=ORIENTED_EDGE('',*,*,#7803,.F.);
#10830=ORIENTED_EDGE('',*,*,#7806,.F.);
#10831=ORIENTED_EDGE('',*,*,#7818,.F.);
#10832=ORIENTED_EDGE('',*,*,#7819,.F.);
#10833=ORIENTED_EDGE('',*,*,#7786,.F.);
#10834=ORIENTED_EDGE('',*,*,#7820,.T.);
#10835=ORIENTED_EDGE('',*,*,#7821,.T.);
#10836=ORIENTED_EDGE('',*,*,#7791,.F.);
#10837=ORIENTED_EDGE('',*,*,#7781,.F.);
#10838=ORIENTED_EDGE('',*,*,#7790,.T.);
#10839=ORIENTED_EDGE('',*,*,#7822,.T.);
#10840=ORIENTED_EDGE('',*,*,#7820,.F.);
#10841=ORIENTED_EDGE('',*,*,#7813,.T.);
#10842=ORIENTED_EDGE('',*,*,#7789,.F.);
#10843=ORIENTED_EDGE('',*,*,#7792,.F.);
#10844=ORIENTED_EDGE('',*,*,#7821,.F.);
#10845=ORIENTED_EDGE('',*,*,#7822,.F.);
#10846=ORIENTED_EDGE('',*,*,#7772,.F.);
#10847=ORIENTED_EDGE('',*,*,#7823,.T.);
#10848=ORIENTED_EDGE('',*,*,#7824,.T.);
#10849=ORIENTED_EDGE('',*,*,#7777,.F.);
#10850=ORIENTED_EDGE('',*,*,#7767,.F.);
#10851=ORIENTED_EDGE('',*,*,#7776,.T.);
#10852=ORIENTED_EDGE('',*,*,#7825,.T.);
#10853=ORIENTED_EDGE('',*,*,#7823,.F.);
#10854=ORIENTED_EDGE('',*,*,#7811,.T.);
#10855=ORIENTED_EDGE('',*,*,#7775,.F.);
#10856=ORIENTED_EDGE('',*,*,#7778,.F.);
#10857=ORIENTED_EDGE('',*,*,#7824,.F.);
#10858=ORIENTED_EDGE('',*,*,#7825,.F.);
#10859=ORIENTED_EDGE('',*,*,#7758,.F.);
#10860=ORIENTED_EDGE('',*,*,#7826,.T.);
#10861=ORIENTED_EDGE('',*,*,#7827,.T.);
#10862=ORIENTED_EDGE('',*,*,#7763,.F.);
#10863=ORIENTED_EDGE('',*,*,#7753,.F.);
#10864=ORIENTED_EDGE('',*,*,#7762,.T.);
#10865=ORIENTED_EDGE('',*,*,#7828,.T.);
#10866=ORIENTED_EDGE('',*,*,#7826,.F.);
#10867=ORIENTED_EDGE('',*,*,#7809,.T.);
#10868=ORIENTED_EDGE('',*,*,#7761,.F.);
#10869=ORIENTED_EDGE('',*,*,#7764,.F.);
#10870=ORIENTED_EDGE('',*,*,#7827,.F.);
#10871=ORIENTED_EDGE('',*,*,#7828,.F.);
#10872=ORIENTED_EDGE('',*,*,#7686,.F.);
#10873=ORIENTED_EDGE('',*,*,#7829,.T.);
#10874=ORIENTED_EDGE('',*,*,#7738,.F.);
#10875=ORIENTED_EDGE('',*,*,#7687,.F.);
#10876=ORIENTED_EDGE('',*,*,#7685,.F.);
#10877=ORIENTED_EDGE('',*,*,#7657,.T.);
#10878=ORIENTED_EDGE('',*,*,#7735,.F.);
#10879=ORIENTED_EDGE('',*,*,#7829,.F.);
#10880=ORIENTED_EDGE('',*,*,#7597,.F.);
#10881=ORIENTED_EDGE('',*,*,#7606,.F.);
#10882=ORIENTED_EDGE('',*,*,#7651,.T.);
#10883=ORIENTED_EDGE('',*,*,#7601,.F.);
#10884=ORIENTED_EDGE('',*,*,#7604,.F.);
#10885=ORIENTED_EDGE('',*,*,#7569,.F.);
#10886=ORIENTED_EDGE('',*,*,#7644,.T.);
#10887=ORIENTED_EDGE('',*,*,#7564,.F.);
#10888=ORIENTED_EDGE('',*,*,#7567,.F.);
#10889=ORIENTED_EDGE('',*,*,#7714,.F.);
#10890=ORIENTED_EDGE('',*,*,#7620,.F.);
#10891=ORIENTED_EDGE('',*,*,#7830,.F.);
#10892=ORIENTED_EDGE('',*,*,#7574,.T.);
#10893=ORIENTED_EDGE('',*,*,#7670,.F.);
#10894=ORIENTED_EDGE('',*,*,#7612,.T.);
#10895=ORIENTED_EDGE('',*,*,#7715,.T.);
#10896=ORIENTED_EDGE('',*,*,#7582,.T.);
#10897=ORIENTED_EDGE('',*,*,#7660,.F.);
#10898=ORIENTED_EDGE('',*,*,#7662,.F.);
#10899=ORIENTED_EDGE('',*,*,#7665,.F.);
#10900=ORIENTED_EDGE('',*,*,#7668,.F.);
#10901=ORIENTED_EDGE('',*,*,#7634,.F.);
#10902=ORIENTED_EDGE('',*,*,#7575,.T.);
#10903=ORIENTED_EDGE('',*,*,#7830,.T.);
#10904=ORIENTED_EDGE('',*,*,#7619,.T.);
#10905=ORIENTED_EDGE('',*,*,#7624,.F.);
#10906=ORIENTED_EDGE('',*,*,#7626,.F.);
#10907=ORIENTED_EDGE('',*,*,#7629,.F.);
#10908=ORIENTED_EDGE('',*,*,#7632,.F.);
#10909=ORIENTED_EDGE('',*,*,#7831,.T.);
#10910=ORIENTED_EDGE('',*,*,#7832,.T.);
#10911=ORIENTED_EDGE('',*,*,#7833,.T.);
#10912=ORIENTED_EDGE('',*,*,#7834,.T.);
#10913=ORIENTED_EDGE('',*,*,#7832,.F.);
#10914=ORIENTED_EDGE('',*,*,#7833,.F.);
#10915=ORIENTED_EDGE('',*,*,#7834,.F.);
#10916=ORIENTED_EDGE('',*,*,#7835,.T.);
#10917=ORIENTED_EDGE('',*,*,#7836,.F.);
#10918=ORIENTED_EDGE('',*,*,#7837,.F.);
#10919=ORIENTED_EDGE('',*,*,#7835,.F.);
#10920=ORIENTED_EDGE('',*,*,#7831,.F.);
#10921=ORIENTED_EDGE('',*,*,#7836,.T.);
#10922=ORIENTED_EDGE('',*,*,#7837,.T.);
#10923=ORIENTED_EDGE('',*,*,#7838,.T.);
#10924=ORIENTED_EDGE('',*,*,#7839,.T.);
#10925=ORIENTED_EDGE('',*,*,#7840,.T.);
#10926=ORIENTED_EDGE('',*,*,#7838,.F.);
#10927=ORIENTED_EDGE('',*,*,#7839,.F.);
#10928=ORIENTED_EDGE('',*,*,#7840,.F.);
#10929=ORIENTED_EDGE('',*,*,#7841,.T.);
#10930=ORIENTED_EDGE('',*,*,#7842,.T.);
#10931=ORIENTED_EDGE('',*,*,#7841,.F.);
#10932=ORIENTED_EDGE('',*,*,#7843,.F.);
#10933=ORIENTED_EDGE('',*,*,#7842,.F.);
#10934=ORIENTED_EDGE('',*,*,#7844,.T.);
#10935=ORIENTED_EDGE('',*,*,#7843,.T.);
#10936=ORIENTED_EDGE('',*,*,#7844,.F.);
#10937=ORIENTED_EDGE('',*,*,#7845,.F.);
#10938=ORIENTED_EDGE('',*,*,#7846,.F.);
#10939=ORIENTED_EDGE('',*,*,#7847,.T.);
#10940=ORIENTED_EDGE('',*,*,#7845,.T.);
#10941=ORIENTED_EDGE('',*,*,#7847,.F.);
#10942=ORIENTED_EDGE('',*,*,#7848,.F.);
#10943=ORIENTED_EDGE('',*,*,#7849,.T.);
#10944=ORIENTED_EDGE('',*,*,#7846,.T.);
#10945=ORIENTED_EDGE('',*,*,#7849,.F.);
#10946=ORIENTED_EDGE('',*,*,#7850,.F.);
#10947=ORIENTED_EDGE('',*,*,#7851,.T.);
#10948=ORIENTED_EDGE('',*,*,#7848,.T.);
#10949=ORIENTED_EDGE('',*,*,#7851,.F.);
#10950=ORIENTED_EDGE('',*,*,#7850,.T.);
#10951=ORIENTED_EDGE('',*,*,#7852,.T.);
#10952=ORIENTED_EDGE('',*,*,#7853,.T.);
#10953=ORIENTED_EDGE('',*,*,#7854,.F.);
#10954=ORIENTED_EDGE('',*,*,#7855,.F.);
#10955=ORIENTED_EDGE('',*,*,#7856,.T.);
#10956=ORIENTED_EDGE('',*,*,#7855,.T.);
#10957=ORIENTED_EDGE('',*,*,#7857,.F.);
#10958=ORIENTED_EDGE('',*,*,#7858,.F.);
#10959=ORIENTED_EDGE('',*,*,#7859,.T.);
#10960=ORIENTED_EDGE('',*,*,#7858,.T.);
#10961=ORIENTED_EDGE('',*,*,#7860,.F.);
#10962=ORIENTED_EDGE('',*,*,#7861,.F.);
#10963=ORIENTED_EDGE('',*,*,#7862,.T.);
#10964=ORIENTED_EDGE('',*,*,#7861,.T.);
#10965=ORIENTED_EDGE('',*,*,#7863,.F.);
#10966=ORIENTED_EDGE('',*,*,#7864,.F.);
#10967=ORIENTED_EDGE('',*,*,#7865,.T.);
#10968=ORIENTED_EDGE('',*,*,#7864,.T.);
#10969=ORIENTED_EDGE('',*,*,#7866,.F.);
#10970=ORIENTED_EDGE('',*,*,#7867,.F.);
#10971=ORIENTED_EDGE('',*,*,#7868,.T.);
#10972=ORIENTED_EDGE('',*,*,#7867,.T.);
#10973=ORIENTED_EDGE('',*,*,#7869,.F.);
#10974=ORIENTED_EDGE('',*,*,#7870,.F.);
#10975=ORIENTED_EDGE('',*,*,#7871,.T.);
#10976=ORIENTED_EDGE('',*,*,#7870,.T.);
#10977=ORIENTED_EDGE('',*,*,#7872,.F.);
#10978=ORIENTED_EDGE('',*,*,#7873,.F.);
#10979=ORIENTED_EDGE('',*,*,#7874,.T.);
#10980=ORIENTED_EDGE('',*,*,#7873,.T.);
#10981=ORIENTED_EDGE('',*,*,#7875,.F.);
#10982=ORIENTED_EDGE('',*,*,#7876,.F.);
#10983=ORIENTED_EDGE('',*,*,#7877,.T.);
#10984=ORIENTED_EDGE('',*,*,#7876,.T.);
#10985=ORIENTED_EDGE('',*,*,#7878,.F.);
#10986=ORIENTED_EDGE('',*,*,#7879,.F.);
#10987=ORIENTED_EDGE('',*,*,#7880,.T.);
#10988=ORIENTED_EDGE('',*,*,#7879,.T.);
#10989=ORIENTED_EDGE('',*,*,#7881,.F.);
#10990=ORIENTED_EDGE('',*,*,#7882,.F.);
#10991=ORIENTED_EDGE('',*,*,#7883,.T.);
#10992=ORIENTED_EDGE('',*,*,#7882,.T.);
#10993=ORIENTED_EDGE('',*,*,#7884,.F.);
#10994=ORIENTED_EDGE('',*,*,#7885,.F.);
#10995=ORIENTED_EDGE('',*,*,#7886,.T.);
#10996=ORIENTED_EDGE('',*,*,#7885,.T.);
#10997=ORIENTED_EDGE('',*,*,#7887,.F.);
#10998=ORIENTED_EDGE('',*,*,#7888,.F.);
#10999=ORIENTED_EDGE('',*,*,#7889,.T.);
#11000=ORIENTED_EDGE('',*,*,#7888,.T.);
#11001=ORIENTED_EDGE('',*,*,#7890,.F.);
#11002=ORIENTED_EDGE('',*,*,#7891,.F.);
#11003=ORIENTED_EDGE('',*,*,#7892,.T.);
#11004=ORIENTED_EDGE('',*,*,#7891,.T.);
#11005=ORIENTED_EDGE('',*,*,#7893,.F.);
#11006=ORIENTED_EDGE('',*,*,#7894,.F.);
#11007=ORIENTED_EDGE('',*,*,#7895,.T.);
#11008=ORIENTED_EDGE('',*,*,#7894,.T.);
#11009=ORIENTED_EDGE('',*,*,#7896,.F.);
#11010=ORIENTED_EDGE('',*,*,#7897,.F.);
#11011=ORIENTED_EDGE('',*,*,#7898,.T.);
#11012=ORIENTED_EDGE('',*,*,#7897,.T.);
#11013=ORIENTED_EDGE('',*,*,#7899,.F.);
#11014=ORIENTED_EDGE('',*,*,#7900,.F.);
#11015=ORIENTED_EDGE('',*,*,#7901,.T.);
#11016=ORIENTED_EDGE('',*,*,#7900,.T.);
#11017=ORIENTED_EDGE('',*,*,#7902,.F.);
#11018=ORIENTED_EDGE('',*,*,#7903,.F.);
#11019=ORIENTED_EDGE('',*,*,#7904,.T.);
#11020=ORIENTED_EDGE('',*,*,#7903,.T.);
#11021=ORIENTED_EDGE('',*,*,#7905,.F.);
#11022=ORIENTED_EDGE('',*,*,#7906,.F.);
#11023=ORIENTED_EDGE('',*,*,#7907,.T.);
#11024=ORIENTED_EDGE('',*,*,#7906,.T.);
#11025=ORIENTED_EDGE('',*,*,#7908,.F.);
#11026=ORIENTED_EDGE('',*,*,#7909,.F.);
#11027=ORIENTED_EDGE('',*,*,#7910,.T.);
#11028=ORIENTED_EDGE('',*,*,#7909,.T.);
#11029=ORIENTED_EDGE('',*,*,#7911,.F.);
#11030=ORIENTED_EDGE('',*,*,#7912,.F.);
#11031=ORIENTED_EDGE('',*,*,#7913,.T.);
#11032=ORIENTED_EDGE('',*,*,#7912,.T.);
#11033=ORIENTED_EDGE('',*,*,#7914,.F.);
#11034=ORIENTED_EDGE('',*,*,#7915,.F.);
#11035=ORIENTED_EDGE('',*,*,#7916,.T.);
#11036=ORIENTED_EDGE('',*,*,#7915,.T.);
#11037=ORIENTED_EDGE('',*,*,#7917,.F.);
#11038=ORIENTED_EDGE('',*,*,#7918,.F.);
#11039=ORIENTED_EDGE('',*,*,#7919,.T.);
#11040=ORIENTED_EDGE('',*,*,#7918,.T.);
#11041=ORIENTED_EDGE('',*,*,#7920,.F.);
#11042=ORIENTED_EDGE('',*,*,#7921,.F.);
#11043=ORIENTED_EDGE('',*,*,#7922,.T.);
#11044=ORIENTED_EDGE('',*,*,#7921,.T.);
#11045=ORIENTED_EDGE('',*,*,#7923,.F.);
#11046=ORIENTED_EDGE('',*,*,#7924,.F.);
#11047=ORIENTED_EDGE('',*,*,#7925,.T.);
#11048=ORIENTED_EDGE('',*,*,#7924,.T.);
#11049=ORIENTED_EDGE('',*,*,#7926,.F.);
#11050=ORIENTED_EDGE('',*,*,#7927,.F.);
#11051=ORIENTED_EDGE('',*,*,#7928,.T.);
#11052=ORIENTED_EDGE('',*,*,#7927,.T.);
#11053=ORIENTED_EDGE('',*,*,#7929,.F.);
#11054=ORIENTED_EDGE('',*,*,#7930,.F.);
#11055=ORIENTED_EDGE('',*,*,#7931,.T.);
#11056=ORIENTED_EDGE('',*,*,#7930,.T.);
#11057=ORIENTED_EDGE('',*,*,#7932,.F.);
#11058=ORIENTED_EDGE('',*,*,#7933,.F.);
#11059=ORIENTED_EDGE('',*,*,#7934,.T.);
#11060=ORIENTED_EDGE('',*,*,#7933,.T.);
#11061=ORIENTED_EDGE('',*,*,#7935,.F.);
#11062=ORIENTED_EDGE('',*,*,#7936,.F.);
#11063=ORIENTED_EDGE('',*,*,#7937,.T.);
#11064=ORIENTED_EDGE('',*,*,#7936,.T.);
#11065=ORIENTED_EDGE('',*,*,#7938,.F.);
#11066=ORIENTED_EDGE('',*,*,#7939,.F.);
#11067=ORIENTED_EDGE('',*,*,#7940,.T.);
#11068=ORIENTED_EDGE('',*,*,#7939,.T.);
#11069=ORIENTED_EDGE('',*,*,#7941,.F.);
#11070=ORIENTED_EDGE('',*,*,#7942,.F.);
#11071=ORIENTED_EDGE('',*,*,#7943,.T.);
#11072=ORIENTED_EDGE('',*,*,#7942,.T.);
#11073=ORIENTED_EDGE('',*,*,#7944,.F.);
#11074=ORIENTED_EDGE('',*,*,#7945,.F.);
#11075=ORIENTED_EDGE('',*,*,#7946,.T.);
#11076=ORIENTED_EDGE('',*,*,#7945,.T.);
#11077=ORIENTED_EDGE('',*,*,#7947,.F.);
#11078=ORIENTED_EDGE('',*,*,#7948,.F.);
#11079=ORIENTED_EDGE('',*,*,#7949,.T.);
#11080=ORIENTED_EDGE('',*,*,#7948,.T.);
#11081=ORIENTED_EDGE('',*,*,#7950,.F.);
#11082=ORIENTED_EDGE('',*,*,#7951,.F.);
#11083=ORIENTED_EDGE('',*,*,#7952,.T.);
#11084=ORIENTED_EDGE('',*,*,#7951,.T.);
#11085=ORIENTED_EDGE('',*,*,#7953,.F.);
#11086=ORIENTED_EDGE('',*,*,#7954,.F.);
#11087=ORIENTED_EDGE('',*,*,#7955,.T.);
#11088=ORIENTED_EDGE('',*,*,#7954,.T.);
#11089=ORIENTED_EDGE('',*,*,#7956,.F.);
#11090=ORIENTED_EDGE('',*,*,#7957,.F.);
#11091=ORIENTED_EDGE('',*,*,#7958,.T.);
#11092=ORIENTED_EDGE('',*,*,#7957,.T.);
#11093=ORIENTED_EDGE('',*,*,#7959,.F.);
#11094=ORIENTED_EDGE('',*,*,#7960,.F.);
#11095=ORIENTED_EDGE('',*,*,#7961,.T.);
#11096=ORIENTED_EDGE('',*,*,#7960,.T.);
#11097=ORIENTED_EDGE('',*,*,#7962,.F.);
#11098=ORIENTED_EDGE('',*,*,#7963,.F.);
#11099=ORIENTED_EDGE('',*,*,#7964,.T.);
#11100=ORIENTED_EDGE('',*,*,#7963,.T.);
#11101=ORIENTED_EDGE('',*,*,#7965,.F.);
#11102=ORIENTED_EDGE('',*,*,#7966,.F.);
#11103=ORIENTED_EDGE('',*,*,#7967,.T.);
#11104=ORIENTED_EDGE('',*,*,#7966,.T.);
#11105=ORIENTED_EDGE('',*,*,#7968,.F.);
#11106=ORIENTED_EDGE('',*,*,#7969,.F.);
#11107=ORIENTED_EDGE('',*,*,#7970,.T.);
#11108=ORIENTED_EDGE('',*,*,#7969,.T.);
#11109=ORIENTED_EDGE('',*,*,#7971,.F.);
#11110=ORIENTED_EDGE('',*,*,#7972,.F.);
#11111=ORIENTED_EDGE('',*,*,#7973,.T.);
#11112=ORIENTED_EDGE('',*,*,#7972,.T.);
#11113=ORIENTED_EDGE('',*,*,#7974,.F.);
#11114=ORIENTED_EDGE('',*,*,#7975,.F.);
#11115=ORIENTED_EDGE('',*,*,#7976,.T.);
#11116=ORIENTED_EDGE('',*,*,#7975,.T.);
#11117=ORIENTED_EDGE('',*,*,#7977,.F.);
#11118=ORIENTED_EDGE('',*,*,#7978,.F.);
#11119=ORIENTED_EDGE('',*,*,#7979,.T.);
#11120=ORIENTED_EDGE('',*,*,#7978,.T.);
#11121=ORIENTED_EDGE('',*,*,#7980,.F.);
#11122=ORIENTED_EDGE('',*,*,#7981,.F.);
#11123=ORIENTED_EDGE('',*,*,#7982,.T.);
#11124=ORIENTED_EDGE('',*,*,#7981,.T.);
#11125=ORIENTED_EDGE('',*,*,#7983,.F.);
#11126=ORIENTED_EDGE('',*,*,#7984,.F.);
#11127=ORIENTED_EDGE('',*,*,#7985,.T.);
#11128=ORIENTED_EDGE('',*,*,#7984,.T.);
#11129=ORIENTED_EDGE('',*,*,#7986,.F.);
#11130=ORIENTED_EDGE('',*,*,#7987,.F.);
#11131=ORIENTED_EDGE('',*,*,#7988,.T.);
#11132=ORIENTED_EDGE('',*,*,#7987,.T.);
#11133=ORIENTED_EDGE('',*,*,#7989,.F.);
#11134=ORIENTED_EDGE('',*,*,#7990,.F.);
#11135=ORIENTED_EDGE('',*,*,#7991,.T.);
#11136=ORIENTED_EDGE('',*,*,#7990,.T.);
#11137=ORIENTED_EDGE('',*,*,#7992,.F.);
#11138=ORIENTED_EDGE('',*,*,#7993,.F.);
#11139=ORIENTED_EDGE('',*,*,#7994,.T.);
#11140=ORIENTED_EDGE('',*,*,#7993,.T.);
#11141=ORIENTED_EDGE('',*,*,#7995,.F.);
#11142=ORIENTED_EDGE('',*,*,#7996,.F.);
#11143=ORIENTED_EDGE('',*,*,#7997,.T.);
#11144=ORIENTED_EDGE('',*,*,#7996,.T.);
#11145=ORIENTED_EDGE('',*,*,#7998,.F.);
#11146=ORIENTED_EDGE('',*,*,#7999,.F.);
#11147=ORIENTED_EDGE('',*,*,#8000,.T.);
#11148=ORIENTED_EDGE('',*,*,#7999,.T.);
#11149=ORIENTED_EDGE('',*,*,#8001,.F.);
#11150=ORIENTED_EDGE('',*,*,#7853,.F.);
#11151=ORIENTED_EDGE('',*,*,#8001,.T.);
#11152=ORIENTED_EDGE('',*,*,#7998,.T.);
#11153=ORIENTED_EDGE('',*,*,#7995,.T.);
#11154=ORIENTED_EDGE('',*,*,#7992,.T.);
#11155=ORIENTED_EDGE('',*,*,#7989,.T.);
#11156=ORIENTED_EDGE('',*,*,#7986,.T.);
#11157=ORIENTED_EDGE('',*,*,#7983,.T.);
#11158=ORIENTED_EDGE('',*,*,#7980,.T.);
#11159=ORIENTED_EDGE('',*,*,#7977,.T.);
#11160=ORIENTED_EDGE('',*,*,#7974,.T.);
#11161=ORIENTED_EDGE('',*,*,#7971,.T.);
#11162=ORIENTED_EDGE('',*,*,#7968,.T.);
#11163=ORIENTED_EDGE('',*,*,#7965,.T.);
#11164=ORIENTED_EDGE('',*,*,#7962,.T.);
#11165=ORIENTED_EDGE('',*,*,#7959,.T.);
#11166=ORIENTED_EDGE('',*,*,#7956,.T.);
#11167=ORIENTED_EDGE('',*,*,#7953,.T.);
#11168=ORIENTED_EDGE('',*,*,#7950,.T.);
#11169=ORIENTED_EDGE('',*,*,#7947,.T.);
#11170=ORIENTED_EDGE('',*,*,#7944,.T.);
#11171=ORIENTED_EDGE('',*,*,#7941,.T.);
#11172=ORIENTED_EDGE('',*,*,#7938,.T.);
#11173=ORIENTED_EDGE('',*,*,#7935,.T.);
#11174=ORIENTED_EDGE('',*,*,#7932,.T.);
#11175=ORIENTED_EDGE('',*,*,#7929,.T.);
#11176=ORIENTED_EDGE('',*,*,#7926,.T.);
#11177=ORIENTED_EDGE('',*,*,#7923,.T.);
#11178=ORIENTED_EDGE('',*,*,#7920,.T.);
#11179=ORIENTED_EDGE('',*,*,#7917,.T.);
#11180=ORIENTED_EDGE('',*,*,#7914,.T.);
#11181=ORIENTED_EDGE('',*,*,#7911,.T.);
#11182=ORIENTED_EDGE('',*,*,#7908,.T.);
#11183=ORIENTED_EDGE('',*,*,#7905,.T.);
#11184=ORIENTED_EDGE('',*,*,#7902,.T.);
#11185=ORIENTED_EDGE('',*,*,#7899,.T.);
#11186=ORIENTED_EDGE('',*,*,#7896,.T.);
#11187=ORIENTED_EDGE('',*,*,#7893,.T.);
#11188=ORIENTED_EDGE('',*,*,#7890,.T.);
#11189=ORIENTED_EDGE('',*,*,#7887,.T.);
#11190=ORIENTED_EDGE('',*,*,#7884,.T.);
#11191=ORIENTED_EDGE('',*,*,#7881,.T.);
#11192=ORIENTED_EDGE('',*,*,#7878,.T.);
#11193=ORIENTED_EDGE('',*,*,#7875,.T.);
#11194=ORIENTED_EDGE('',*,*,#7872,.T.);
#11195=ORIENTED_EDGE('',*,*,#7869,.T.);
#11196=ORIENTED_EDGE('',*,*,#7866,.T.);
#11197=ORIENTED_EDGE('',*,*,#7863,.T.);
#11198=ORIENTED_EDGE('',*,*,#7860,.T.);
#11199=ORIENTED_EDGE('',*,*,#7857,.T.);
#11200=ORIENTED_EDGE('',*,*,#7854,.T.);
#11201=ORIENTED_EDGE('',*,*,#8000,.F.);
#11202=ORIENTED_EDGE('',*,*,#7852,.F.);
#11203=ORIENTED_EDGE('',*,*,#7856,.F.);
#11204=ORIENTED_EDGE('',*,*,#7859,.F.);
#11205=ORIENTED_EDGE('',*,*,#7862,.F.);
#11206=ORIENTED_EDGE('',*,*,#7865,.F.);
#11207=ORIENTED_EDGE('',*,*,#7868,.F.);
#11208=ORIENTED_EDGE('',*,*,#7871,.F.);
#11209=ORIENTED_EDGE('',*,*,#7874,.F.);
#11210=ORIENTED_EDGE('',*,*,#7877,.F.);
#11211=ORIENTED_EDGE('',*,*,#7880,.F.);
#11212=ORIENTED_EDGE('',*,*,#7883,.F.);
#11213=ORIENTED_EDGE('',*,*,#7886,.F.);
#11214=ORIENTED_EDGE('',*,*,#7889,.F.);
#11215=ORIENTED_EDGE('',*,*,#7892,.F.);
#11216=ORIENTED_EDGE('',*,*,#7895,.F.);
#11217=ORIENTED_EDGE('',*,*,#7898,.F.);
#11218=ORIENTED_EDGE('',*,*,#7901,.F.);
#11219=ORIENTED_EDGE('',*,*,#7904,.F.);
#11220=ORIENTED_EDGE('',*,*,#7907,.F.);
#11221=ORIENTED_EDGE('',*,*,#7910,.F.);
#11222=ORIENTED_EDGE('',*,*,#7913,.F.);
#11223=ORIENTED_EDGE('',*,*,#7916,.F.);
#11224=ORIENTED_EDGE('',*,*,#7919,.F.);
#11225=ORIENTED_EDGE('',*,*,#7922,.F.);
#11226=ORIENTED_EDGE('',*,*,#7925,.F.);
#11227=ORIENTED_EDGE('',*,*,#7928,.F.);
#11228=ORIENTED_EDGE('',*,*,#7931,.F.);
#11229=ORIENTED_EDGE('',*,*,#7934,.F.);
#11230=ORIENTED_EDGE('',*,*,#7937,.F.);
#11231=ORIENTED_EDGE('',*,*,#7940,.F.);
#11232=ORIENTED_EDGE('',*,*,#7943,.F.);
#11233=ORIENTED_EDGE('',*,*,#7946,.F.);
#11234=ORIENTED_EDGE('',*,*,#7949,.F.);
#11235=ORIENTED_EDGE('',*,*,#7952,.F.);
#11236=ORIENTED_EDGE('',*,*,#7955,.F.);
#11237=ORIENTED_EDGE('',*,*,#7958,.F.);
#11238=ORIENTED_EDGE('',*,*,#7961,.F.);
#11239=ORIENTED_EDGE('',*,*,#7964,.F.);
#11240=ORIENTED_EDGE('',*,*,#7967,.F.);
#11241=ORIENTED_EDGE('',*,*,#7970,.F.);
#11242=ORIENTED_EDGE('',*,*,#7973,.F.);
#11243=ORIENTED_EDGE('',*,*,#7976,.F.);
#11244=ORIENTED_EDGE('',*,*,#7979,.F.);
#11245=ORIENTED_EDGE('',*,*,#7982,.F.);
#11246=ORIENTED_EDGE('',*,*,#7985,.F.);
#11247=ORIENTED_EDGE('',*,*,#7988,.F.);
#11248=ORIENTED_EDGE('',*,*,#7991,.F.);
#11249=ORIENTED_EDGE('',*,*,#7994,.F.);
#11250=ORIENTED_EDGE('',*,*,#7997,.F.);
#11251=ORIENTED_EDGE('',*,*,#8002,.T.);
#11252=ORIENTED_EDGE('',*,*,#8003,.T.);
#11253=ORIENTED_EDGE('',*,*,#8004,.T.);
#11254=ORIENTED_EDGE('',*,*,#8005,.T.);
#11255=ORIENTED_EDGE('',*,*,#8006,.T.);
#11256=ORIENTED_EDGE('',*,*,#8007,.T.);
#11257=ORIENTED_EDGE('',*,*,#8002,.F.);
#11258=ORIENTED_EDGE('',*,*,#8008,.T.);
#11259=ORIENTED_EDGE('',*,*,#8009,.T.);
#11260=ORIENTED_EDGE('',*,*,#8010,.T.);
#11261=ORIENTED_EDGE('',*,*,#8006,.F.);
#11262=ORIENTED_EDGE('',*,*,#8011,.T.);
#11263=ORIENTED_EDGE('',*,*,#8012,.T.);
#11264=ORIENTED_EDGE('',*,*,#8013,.T.);
#11265=ORIENTED_EDGE('',*,*,#8009,.F.);
#11266=ORIENTED_EDGE('',*,*,#8014,.T.);
#11267=ORIENTED_EDGE('',*,*,#8015,.T.);
#11268=ORIENTED_EDGE('',*,*,#8016,.T.);
#11269=ORIENTED_EDGE('',*,*,#8012,.F.);
#11270=ORIENTED_EDGE('',*,*,#8017,.T.);
#11271=ORIENTED_EDGE('',*,*,#8018,.T.);
#11272=ORIENTED_EDGE('',*,*,#8019,.T.);
#11273=ORIENTED_EDGE('',*,*,#8015,.F.);
#11274=ORIENTED_EDGE('',*,*,#8020,.T.);
#11275=ORIENTED_EDGE('',*,*,#8021,.T.);
#11276=ORIENTED_EDGE('',*,*,#8022,.T.);
#11277=ORIENTED_EDGE('',*,*,#8018,.F.);
#11278=ORIENTED_EDGE('',*,*,#8023,.T.);
#11279=ORIENTED_EDGE('',*,*,#8004,.F.);
#11280=ORIENTED_EDGE('',*,*,#8024,.T.);
#11281=ORIENTED_EDGE('',*,*,#8021,.F.);
#11282=ORIENTED_EDGE('',*,*,#8025,.T.);
#11283=ORIENTED_EDGE('',*,*,#8014,.F.);
#11284=ORIENTED_EDGE('',*,*,#8026,.T.);
#11285=ORIENTED_EDGE('',*,*,#8027,.F.);
#11286=ORIENTED_EDGE('',*,*,#8028,.F.);
#11287=ORIENTED_EDGE('',*,*,#8011,.F.);
#11288=ORIENTED_EDGE('',*,*,#8029,.T.);
#11289=ORIENTED_EDGE('',*,*,#8030,.F.);
#11290=ORIENTED_EDGE('',*,*,#8026,.F.);
#11291=ORIENTED_EDGE('',*,*,#8008,.F.);
#11292=ORIENTED_EDGE('',*,*,#8031,.T.);
#11293=ORIENTED_EDGE('',*,*,#8032,.F.);
#11294=ORIENTED_EDGE('',*,*,#8029,.F.);
#11295=ORIENTED_EDGE('',*,*,#8005,.F.);
#11296=ORIENTED_EDGE('',*,*,#8033,.T.);
#11297=ORIENTED_EDGE('',*,*,#8034,.F.);
#11298=ORIENTED_EDGE('',*,*,#8031,.F.);
#11299=ORIENTED_EDGE('',*,*,#8035,.F.);
#11300=ORIENTED_EDGE('',*,*,#8036,.F.);
#11301=ORIENTED_EDGE('',*,*,#8037,.F.);
#11302=ORIENTED_EDGE('',*,*,#8038,.F.);
#11303=ORIENTED_EDGE('',*,*,#8039,.F.);
#11304=ORIENTED_EDGE('',*,*,#8040,.F.);
#11305=ORIENTED_EDGE('',*,*,#8041,.F.);
#11306=ORIENTED_EDGE('',*,*,#8042,.F.);
#11307=ORIENTED_EDGE('',*,*,#8003,.F.);
#11308=ORIENTED_EDGE('',*,*,#8007,.F.);
#11309=ORIENTED_EDGE('',*,*,#8010,.F.);
#11310=ORIENTED_EDGE('',*,*,#8013,.F.);
#11311=ORIENTED_EDGE('',*,*,#8016,.F.);
#11312=ORIENTED_EDGE('',*,*,#8019,.F.);
#11313=ORIENTED_EDGE('',*,*,#8022,.F.);
#11314=ORIENTED_EDGE('',*,*,#8024,.F.);
#11315=ORIENTED_EDGE('',*,*,#8043,.T.);
#11316=ORIENTED_EDGE('',*,*,#8044,.T.);
#11317=ORIENTED_EDGE('',*,*,#8045,.T.);
#11318=ORIENTED_EDGE('',*,*,#8046,.T.);
#11319=ORIENTED_EDGE('',*,*,#8047,.T.);
#11320=ORIENTED_EDGE('',*,*,#8048,.T.);
#11321=ORIENTED_EDGE('',*,*,#8043,.F.);
#11322=ORIENTED_EDGE('',*,*,#8049,.T.);
#11323=ORIENTED_EDGE('',*,*,#8050,.T.);
#11324=ORIENTED_EDGE('',*,*,#8051,.T.);
#11325=ORIENTED_EDGE('',*,*,#8047,.F.);
#11326=ORIENTED_EDGE('',*,*,#8052,.T.);
#11327=ORIENTED_EDGE('',*,*,#8053,.T.);
#11328=ORIENTED_EDGE('',*,*,#8054,.T.);
#11329=ORIENTED_EDGE('',*,*,#8050,.F.);
#11330=ORIENTED_EDGE('',*,*,#8055,.T.);
#11331=ORIENTED_EDGE('',*,*,#8056,.T.);
#11332=ORIENTED_EDGE('',*,*,#8057,.T.);
#11333=ORIENTED_EDGE('',*,*,#8053,.F.);
#11334=ORIENTED_EDGE('',*,*,#8058,.T.);
#11335=ORIENTED_EDGE('',*,*,#8059,.T.);
#11336=ORIENTED_EDGE('',*,*,#8060,.T.);
#11337=ORIENTED_EDGE('',*,*,#8056,.F.);
#11338=ORIENTED_EDGE('',*,*,#8061,.T.);
#11339=ORIENTED_EDGE('',*,*,#8062,.T.);
#11340=ORIENTED_EDGE('',*,*,#8063,.T.);
#11341=ORIENTED_EDGE('',*,*,#8059,.F.);
#11342=ORIENTED_EDGE('',*,*,#8064,.T.);
#11343=ORIENTED_EDGE('',*,*,#8045,.F.);
#11344=ORIENTED_EDGE('',*,*,#8065,.T.);
#11345=ORIENTED_EDGE('',*,*,#8062,.F.);
#11346=ORIENTED_EDGE('',*,*,#8066,.T.);
#11347=ORIENTED_EDGE('',*,*,#8055,.F.);
#11348=ORIENTED_EDGE('',*,*,#8067,.T.);
#11349=ORIENTED_EDGE('',*,*,#8041,.T.);
#11350=ORIENTED_EDGE('',*,*,#8068,.F.);
#11351=ORIENTED_EDGE('',*,*,#8052,.F.);
#11352=ORIENTED_EDGE('',*,*,#8069,.T.);
#11353=ORIENTED_EDGE('',*,*,#8042,.T.);
#11354=ORIENTED_EDGE('',*,*,#8067,.F.);
#11355=ORIENTED_EDGE('',*,*,#8049,.F.);
#11356=ORIENTED_EDGE('',*,*,#8070,.T.);
#11357=ORIENTED_EDGE('',*,*,#8035,.T.);
#11358=ORIENTED_EDGE('',*,*,#8069,.F.);
#11359=ORIENTED_EDGE('',*,*,#8046,.F.);
#11360=ORIENTED_EDGE('',*,*,#8071,.T.);
#11361=ORIENTED_EDGE('',*,*,#8036,.T.);
#11362=ORIENTED_EDGE('',*,*,#8070,.F.);
#11363=ORIENTED_EDGE('',*,*,#8072,.F.);
#11364=ORIENTED_EDGE('',*,*,#8073,.F.);
#11365=ORIENTED_EDGE('',*,*,#8074,.F.);
#11366=ORIENTED_EDGE('',*,*,#8075,.F.);
#11367=ORIENTED_EDGE('',*,*,#8076,.F.);
#11368=ORIENTED_EDGE('',*,*,#8077,.F.);
#11369=ORIENTED_EDGE('',*,*,#8078,.F.);
#11370=ORIENTED_EDGE('',*,*,#8079,.F.);
#11371=ORIENTED_EDGE('',*,*,#8044,.F.);
#11372=ORIENTED_EDGE('',*,*,#8048,.F.);
#11373=ORIENTED_EDGE('',*,*,#8051,.F.);
#11374=ORIENTED_EDGE('',*,*,#8054,.F.);
#11375=ORIENTED_EDGE('',*,*,#8057,.F.);
#11376=ORIENTED_EDGE('',*,*,#8060,.F.);
#11377=ORIENTED_EDGE('',*,*,#8063,.F.);
#11378=ORIENTED_EDGE('',*,*,#8065,.F.);
#11379=ORIENTED_EDGE('',*,*,#8080,.T.);
#11380=ORIENTED_EDGE('',*,*,#8072,.T.);
#11381=ORIENTED_EDGE('',*,*,#8081,.T.);
#11382=ORIENTED_EDGE('',*,*,#8082,.T.);
#11383=ORIENTED_EDGE('',*,*,#8080,.F.);
#11384=ORIENTED_EDGE('',*,*,#8083,.T.);
#11385=ORIENTED_EDGE('',*,*,#8084,.T.);
#11386=ORIENTED_EDGE('',*,*,#8073,.T.);
#11387=ORIENTED_EDGE('',*,*,#8085,.T.);
#11388=ORIENTED_EDGE('',*,*,#8074,.T.);
#11389=ORIENTED_EDGE('',*,*,#8084,.F.);
#11390=ORIENTED_EDGE('',*,*,#8086,.T.);
#11391=ORIENTED_EDGE('',*,*,#8085,.F.);
#11392=ORIENTED_EDGE('',*,*,#8087,.T.);
#11393=ORIENTED_EDGE('',*,*,#8088,.T.);
#11394=ORIENTED_EDGE('',*,*,#8075,.T.);
#11395=ORIENTED_EDGE('',*,*,#8089,.T.);
#11396=ORIENTED_EDGE('',*,*,#8076,.T.);
#11397=ORIENTED_EDGE('',*,*,#8088,.F.);
#11398=ORIENTED_EDGE('',*,*,#8090,.T.);
#11399=ORIENTED_EDGE('',*,*,#8089,.F.);
#11400=ORIENTED_EDGE('',*,*,#8091,.T.);
#11401=ORIENTED_EDGE('',*,*,#8092,.T.);
#11402=ORIENTED_EDGE('',*,*,#8077,.T.);
#11403=ORIENTED_EDGE('',*,*,#8093,.T.);
#11404=ORIENTED_EDGE('',*,*,#8078,.T.);
#11405=ORIENTED_EDGE('',*,*,#8092,.F.);
#11406=ORIENTED_EDGE('',*,*,#8094,.T.);
#11407=ORIENTED_EDGE('',*,*,#8093,.F.);
#11408=ORIENTED_EDGE('',*,*,#8095,.T.);
#11409=ORIENTED_EDGE('',*,*,#8081,.F.);
#11410=ORIENTED_EDGE('',*,*,#8079,.T.);
#11411=ORIENTED_EDGE('',*,*,#8087,.F.);
#11412=ORIENTED_EDGE('',*,*,#8096,.T.);
#11413=ORIENTED_EDGE('',*,*,#8097,.F.);
#11414=ORIENTED_EDGE('',*,*,#8098,.F.);
#11415=ORIENTED_EDGE('',*,*,#8099,.F.);
#11416=ORIENTED_EDGE('',*,*,#8100,.F.);
#11417=ORIENTED_EDGE('',*,*,#8086,.F.);
#11418=ORIENTED_EDGE('',*,*,#8101,.T.);
#11419=ORIENTED_EDGE('',*,*,#8102,.F.);
#11420=ORIENTED_EDGE('',*,*,#8103,.F.);
#11421=ORIENTED_EDGE('',*,*,#8104,.F.);
#11422=ORIENTED_EDGE('',*,*,#8105,.F.);
#11423=ORIENTED_EDGE('',*,*,#8106,.F.);
#11424=ORIENTED_EDGE('',*,*,#8107,.F.);
#11425=ORIENTED_EDGE('',*,*,#8108,.F.);
#11426=ORIENTED_EDGE('',*,*,#8096,.F.);
#11427=ORIENTED_EDGE('',*,*,#8083,.F.);
#11428=ORIENTED_EDGE('',*,*,#8109,.T.);
#11429=ORIENTED_EDGE('',*,*,#8110,.F.);
#11430=ORIENTED_EDGE('',*,*,#8111,.F.);
#11431=ORIENTED_EDGE('',*,*,#8112,.F.);
#11432=ORIENTED_EDGE('',*,*,#8101,.F.);
#11433=ORIENTED_EDGE('',*,*,#8082,.F.);
#11434=ORIENTED_EDGE('',*,*,#8113,.T.);
#11435=ORIENTED_EDGE('',*,*,#8114,.F.);
#11436=ORIENTED_EDGE('',*,*,#8115,.F.);
#11437=ORIENTED_EDGE('',*,*,#8116,.F.);
#11438=ORIENTED_EDGE('',*,*,#8117,.F.);
#11439=ORIENTED_EDGE('',*,*,#8118,.F.);
#11440=ORIENTED_EDGE('',*,*,#8119,.F.);
#11441=ORIENTED_EDGE('',*,*,#8120,.F.);
#11442=ORIENTED_EDGE('',*,*,#8109,.F.);
#11443=ORIENTED_EDGE('',*,*,#8121,.T.);
#11444=ORIENTED_EDGE('',*,*,#8122,.F.);
#11445=ORIENTED_EDGE('',*,*,#8123,.T.);
#11446=ORIENTED_EDGE('',*,*,#8099,.T.);
#11447=ORIENTED_EDGE('',*,*,#8124,.T.);
#11448=ORIENTED_EDGE('',*,*,#8125,.F.);
#11449=ORIENTED_EDGE('',*,*,#8126,.T.);
#11450=ORIENTED_EDGE('',*,*,#8127,.T.);
#11451=ORIENTED_EDGE('',*,*,#8125,.T.);
#11452=ORIENTED_EDGE('',*,*,#8128,.T.);
#11453=ORIENTED_EDGE('',*,*,#8129,.T.);
#11454=ORIENTED_EDGE('',*,*,#8130,.T.);
#11455=ORIENTED_EDGE('',*,*,#8131,.T.);
#11456=ORIENTED_EDGE('',*,*,#8132,.T.);
#11457=ORIENTED_EDGE('',*,*,#8133,.T.);
#11458=ORIENTED_EDGE('',*,*,#8134,.T.);
#11459=ORIENTED_EDGE('',*,*,#8133,.F.);
#11460=ORIENTED_EDGE('',*,*,#8135,.T.);
#11461=ORIENTED_EDGE('',*,*,#8129,.F.);
#11462=ORIENTED_EDGE('',*,*,#8136,.T.);
#11463=ORIENTED_EDGE('',*,*,#8122,.T.);
#11464=ORIENTED_EDGE('',*,*,#8137,.T.);
#11465=ORIENTED_EDGE('',*,*,#8138,.T.);
#11466=ORIENTED_EDGE('',*,*,#8139,.T.);
#11467=ORIENTED_EDGE('',*,*,#8138,.F.);
#11468=ORIENTED_EDGE('',*,*,#8140,.T.);
#11469=ORIENTED_EDGE('',*,*,#8131,.F.);
#11470=ORIENTED_EDGE('',*,*,#8141,.T.);
#11471=ORIENTED_EDGE('',*,*,#8137,.F.);
#11472=ORIENTED_EDGE('',*,*,#8121,.F.);
#11473=ORIENTED_EDGE('',*,*,#8098,.T.);
#11474=ORIENTED_EDGE('',*,*,#8142,.F.);
#11475=ORIENTED_EDGE('',*,*,#8143,.F.);
#11476=ORIENTED_EDGE('',*,*,#8144,.T.);
#11477=ORIENTED_EDGE('',*,*,#8090,.F.);
#11478=ORIENTED_EDGE('',*,*,#8100,.T.);
#11479=ORIENTED_EDGE('',*,*,#8123,.F.);
#11480=ORIENTED_EDGE('',*,*,#8139,.F.);
#11481=ORIENTED_EDGE('',*,*,#8141,.F.);
#11482=ORIENTED_EDGE('',*,*,#8134,.F.);
#11483=ORIENTED_EDGE('',*,*,#8136,.F.);
#11484=ORIENTED_EDGE('',*,*,#8128,.F.);
#11485=ORIENTED_EDGE('',*,*,#8124,.F.);
#11486=ORIENTED_EDGE('',*,*,#8145,.F.);
#11487=ORIENTED_EDGE('',*,*,#8146,.T.);
#11488=ORIENTED_EDGE('',*,*,#8147,.F.);
#11489=ORIENTED_EDGE('',*,*,#8148,.T.);
#11490=ORIENTED_EDGE('',*,*,#8149,.T.);
#11491=ORIENTED_EDGE('',*,*,#8150,.T.);
#11492=ORIENTED_EDGE('',*,*,#8151,.F.);
#11493=ORIENTED_EDGE('',*,*,#8152,.T.);
#11494=ORIENTED_EDGE('',*,*,#8153,.T.);
#11495=ORIENTED_EDGE('',*,*,#8151,.T.);
#11496=ORIENTED_EDGE('',*,*,#8154,.T.);
#11497=ORIENTED_EDGE('',*,*,#8155,.T.);
#11498=ORIENTED_EDGE('',*,*,#8156,.T.);
#11499=ORIENTED_EDGE('',*,*,#8157,.T.);
#11500=ORIENTED_EDGE('',*,*,#8158,.T.);
#11501=ORIENTED_EDGE('',*,*,#8159,.T.);
#11502=ORIENTED_EDGE('',*,*,#8160,.T.);
#11503=ORIENTED_EDGE('',*,*,#8159,.F.);
#11504=ORIENTED_EDGE('',*,*,#8161,.T.);
#11505=ORIENTED_EDGE('',*,*,#8155,.F.);
#11506=ORIENTED_EDGE('',*,*,#8162,.T.);
#11507=ORIENTED_EDGE('',*,*,#8147,.T.);
#11508=ORIENTED_EDGE('',*,*,#8163,.T.);
#11509=ORIENTED_EDGE('',*,*,#8164,.T.);
#11510=ORIENTED_EDGE('',*,*,#8165,.T.);
#11511=ORIENTED_EDGE('',*,*,#8164,.F.);
#11512=ORIENTED_EDGE('',*,*,#8166,.T.);
#11513=ORIENTED_EDGE('',*,*,#8157,.F.);
#11514=ORIENTED_EDGE('',*,*,#8167,.T.);
#11515=ORIENTED_EDGE('',*,*,#8130,.F.);
#11516=ORIENTED_EDGE('',*,*,#8168,.T.);
#11517=ORIENTED_EDGE('',*,*,#8163,.F.);
#11518=ORIENTED_EDGE('',*,*,#8146,.F.);
#11519=ORIENTED_EDGE('',*,*,#8169,.T.);
#11520=ORIENTED_EDGE('',*,*,#8126,.F.);
#11521=ORIENTED_EDGE('',*,*,#8091,.F.);
#11522=ORIENTED_EDGE('',*,*,#8145,.T.);
#11523=ORIENTED_EDGE('',*,*,#8127,.F.);
#11524=ORIENTED_EDGE('',*,*,#8169,.F.);
#11525=ORIENTED_EDGE('',*,*,#8149,.F.);
#11526=ORIENTED_EDGE('',*,*,#8170,.F.);
#11527=ORIENTED_EDGE('',*,*,#8094,.F.);
#11528=ORIENTED_EDGE('',*,*,#8170,.T.);
#11529=ORIENTED_EDGE('',*,*,#8148,.F.);
#11530=ORIENTED_EDGE('',*,*,#8165,.F.);
#11531=ORIENTED_EDGE('',*,*,#8167,.F.);
#11532=ORIENTED_EDGE('',*,*,#8160,.F.);
#11533=ORIENTED_EDGE('',*,*,#8162,.F.);
#11534=ORIENTED_EDGE('',*,*,#8154,.F.);
#11535=ORIENTED_EDGE('',*,*,#8150,.F.);
#11536=ORIENTED_EDGE('',*,*,#8171,.F.);
#11537=ORIENTED_EDGE('',*,*,#8172,.T.);
#11538=ORIENTED_EDGE('',*,*,#8173,.T.);
#11539=ORIENTED_EDGE('',*,*,#8174,.T.);
#11540=ORIENTED_EDGE('',*,*,#8027,.T.);
#11541=ORIENTED_EDGE('',*,*,#8175,.T.);
#11542=ORIENTED_EDGE('',*,*,#8176,.T.);
#11543=ORIENTED_EDGE('',*,*,#8172,.F.);
#11544=ORIENTED_EDGE('',*,*,#8030,.T.);
#11545=ORIENTED_EDGE('',*,*,#8177,.T.);
#11546=ORIENTED_EDGE('',*,*,#8178,.T.);
#11547=ORIENTED_EDGE('',*,*,#8175,.F.);
#11548=ORIENTED_EDGE('',*,*,#8032,.T.);
#11549=ORIENTED_EDGE('',*,*,#8179,.T.);
#11550=ORIENTED_EDGE('',*,*,#8180,.T.);
#11551=ORIENTED_EDGE('',*,*,#8177,.F.);
#11552=ORIENTED_EDGE('',*,*,#8034,.T.);
#11553=ORIENTED_EDGE('',*,*,#8181,.T.);
#11554=ORIENTED_EDGE('',*,*,#8182,.T.);
#11555=ORIENTED_EDGE('',*,*,#8179,.F.);
#11556=ORIENTED_EDGE('',*,*,#8183,.T.);
#11557=ORIENTED_EDGE('',*,*,#8184,.T.);
#11558=ORIENTED_EDGE('',*,*,#8185,.T.);
#11559=ORIENTED_EDGE('',*,*,#8181,.F.);
#11560=ORIENTED_EDGE('',*,*,#8186,.T.);
#11561=ORIENTED_EDGE('',*,*,#8187,.T.);
#11562=ORIENTED_EDGE('',*,*,#8188,.T.);
#11563=ORIENTED_EDGE('',*,*,#8184,.F.);
#11564=ORIENTED_EDGE('',*,*,#8189,.T.);
#11565=ORIENTED_EDGE('',*,*,#8174,.F.);
#11566=ORIENTED_EDGE('',*,*,#8190,.T.);
#11567=ORIENTED_EDGE('',*,*,#8187,.F.);
#11568=ORIENTED_EDGE('',*,*,#8191,.T.);
#11569=ORIENTED_EDGE('',*,*,#8140,.F.);
#11570=ORIENTED_EDGE('',*,*,#8144,.F.);
#11571=ORIENTED_EDGE('',*,*,#8192,.F.);
#11572=ORIENTED_EDGE('',*,*,#8193,.F.);
#11573=ORIENTED_EDGE('',*,*,#8194,.F.);
#11574=ORIENTED_EDGE('',*,*,#8195,.F.);
#11575=ORIENTED_EDGE('',*,*,#8196,.F.);
#11576=ORIENTED_EDGE('',*,*,#8197,.F.);
#11577=ORIENTED_EDGE('',*,*,#8198,.F.);
#11578=ORIENTED_EDGE('',*,*,#8199,.F.);
#11579=ORIENTED_EDGE('',*,*,#8161,.F.);
#11580=ORIENTED_EDGE('',*,*,#8158,.F.);
#11581=ORIENTED_EDGE('',*,*,#8166,.F.);
#11582=ORIENTED_EDGE('',*,*,#8168,.F.);
#11583=ORIENTED_EDGE('',*,*,#8135,.F.);
#11584=ORIENTED_EDGE('',*,*,#8132,.F.);
#11585=ORIENTED_EDGE('',*,*,#8173,.F.);
#11586=ORIENTED_EDGE('',*,*,#8176,.F.);
#11587=ORIENTED_EDGE('',*,*,#8178,.F.);
#11588=ORIENTED_EDGE('',*,*,#8180,.F.);
#11589=ORIENTED_EDGE('',*,*,#8182,.F.);
#11590=ORIENTED_EDGE('',*,*,#8185,.F.);
#11591=ORIENTED_EDGE('',*,*,#8188,.F.);
#11592=ORIENTED_EDGE('',*,*,#8190,.F.);
#11593=ORIENTED_EDGE('',*,*,#8200,.T.);
#11594=ORIENTED_EDGE('',*,*,#8201,.F.);
#11595=ORIENTED_EDGE('',*,*,#8102,.T.);
#11596=ORIENTED_EDGE('',*,*,#8112,.T.);
#11597=ORIENTED_EDGE('',*,*,#8108,.T.);
#11598=ORIENTED_EDGE('',*,*,#8202,.F.);
#11599=ORIENTED_EDGE('',*,*,#8142,.T.);
#11600=ORIENTED_EDGE('',*,*,#8097,.T.);
#11601=ORIENTED_EDGE('',*,*,#8202,.T.);
#11602=ORIENTED_EDGE('',*,*,#8107,.T.);
#11603=ORIENTED_EDGE('',*,*,#8203,.T.);
#11604=ORIENTED_EDGE('',*,*,#8143,.T.);
#11605=ORIENTED_EDGE('',*,*,#8204,.T.);
#11606=ORIENTED_EDGE('',*,*,#8193,.T.);
#11607=ORIENTED_EDGE('',*,*,#8205,.T.);
#11608=ORIENTED_EDGE('',*,*,#8105,.T.);
#11609=ORIENTED_EDGE('',*,*,#8205,.F.);
#11610=ORIENTED_EDGE('',*,*,#8192,.T.);
#11611=ORIENTED_EDGE('',*,*,#8203,.F.);
#11612=ORIENTED_EDGE('',*,*,#8106,.T.);
#11613=ORIENTED_EDGE('',*,*,#8201,.T.);
#11614=ORIENTED_EDGE('',*,*,#8206,.T.);
#11615=ORIENTED_EDGE('',*,*,#8207,.T.);
#11616=ORIENTED_EDGE('',*,*,#8103,.T.);
#11617=ORIENTED_EDGE('',*,*,#8207,.F.);
#11618=ORIENTED_EDGE('',*,*,#8194,.T.);
#11619=ORIENTED_EDGE('',*,*,#8204,.F.);
#11620=ORIENTED_EDGE('',*,*,#8104,.T.);
#11621=ORIENTED_EDGE('',*,*,#8206,.F.);
#11622=ORIENTED_EDGE('',*,*,#8200,.F.);
#11623=ORIENTED_EDGE('',*,*,#8111,.T.);
#11624=ORIENTED_EDGE('',*,*,#8208,.F.);
#11625=ORIENTED_EDGE('',*,*,#8209,.F.);
#11626=ORIENTED_EDGE('',*,*,#8195,.T.);
#11627=ORIENTED_EDGE('',*,*,#8210,.T.);
#11628=ORIENTED_EDGE('',*,*,#8211,.F.);
#11629=ORIENTED_EDGE('',*,*,#8114,.T.);
#11630=ORIENTED_EDGE('',*,*,#8212,.T.);
#11631=ORIENTED_EDGE('',*,*,#8120,.T.);
#11632=ORIENTED_EDGE('',*,*,#8213,.F.);
#11633=ORIENTED_EDGE('',*,*,#8208,.T.);
#11634=ORIENTED_EDGE('',*,*,#8110,.T.);
#11635=ORIENTED_EDGE('',*,*,#8213,.T.);
#11636=ORIENTED_EDGE('',*,*,#8119,.T.);
#11637=ORIENTED_EDGE('',*,*,#8214,.T.);
#11638=ORIENTED_EDGE('',*,*,#8209,.T.);
#11639=ORIENTED_EDGE('',*,*,#8215,.T.);
#11640=ORIENTED_EDGE('',*,*,#8197,.T.);
#11641=ORIENTED_EDGE('',*,*,#8216,.T.);
#11642=ORIENTED_EDGE('',*,*,#8117,.T.);
#11643=ORIENTED_EDGE('',*,*,#8216,.F.);
#11644=ORIENTED_EDGE('',*,*,#8196,.T.);
#11645=ORIENTED_EDGE('',*,*,#8214,.F.);
#11646=ORIENTED_EDGE('',*,*,#8118,.T.);
#11647=ORIENTED_EDGE('',*,*,#8211,.T.);
#11648=ORIENTED_EDGE('',*,*,#8217,.T.);
#11649=ORIENTED_EDGE('',*,*,#8218,.T.);
#11650=ORIENTED_EDGE('',*,*,#8115,.T.);
#11651=ORIENTED_EDGE('',*,*,#8218,.F.);
#11652=ORIENTED_EDGE('',*,*,#8198,.T.);
#11653=ORIENTED_EDGE('',*,*,#8215,.F.);
#11654=ORIENTED_EDGE('',*,*,#8116,.T.);
#11655=ORIENTED_EDGE('',*,*,#8156,.F.);
#11656=ORIENTED_EDGE('',*,*,#8199,.T.);
#11657=ORIENTED_EDGE('',*,*,#8217,.F.);
#11658=ORIENTED_EDGE('',*,*,#8210,.F.);
#11659=ORIENTED_EDGE('',*,*,#8219,.T.);
#11660=ORIENTED_EDGE('',*,*,#8152,.F.);
#11661=ORIENTED_EDGE('',*,*,#8095,.F.);
#11662=ORIENTED_EDGE('',*,*,#8171,.T.);
#11663=ORIENTED_EDGE('',*,*,#8153,.F.);
#11664=ORIENTED_EDGE('',*,*,#8219,.F.);
#11665=ORIENTED_EDGE('',*,*,#8212,.F.);
#11666=ORIENTED_EDGE('',*,*,#8113,.F.);
#11667=ORIENTED_EDGE('',*,*,#8017,.F.);
#11668=ORIENTED_EDGE('',*,*,#8028,.T.);
#11669=ORIENTED_EDGE('',*,*,#8191,.F.);
#11670=ORIENTED_EDGE('',*,*,#8220,.F.);
#11671=ORIENTED_EDGE('',*,*,#8020,.F.);
#11672=ORIENTED_EDGE('',*,*,#8220,.T.);
#11673=ORIENTED_EDGE('',*,*,#8189,.F.);
#11674=ORIENTED_EDGE('',*,*,#8221,.F.);
#11675=ORIENTED_EDGE('',*,*,#8023,.F.);
#11676=ORIENTED_EDGE('',*,*,#8221,.T.);
#11677=ORIENTED_EDGE('',*,*,#8186,.F.);
#11678=ORIENTED_EDGE('',*,*,#8222,.F.);
#11679=ORIENTED_EDGE('',*,*,#8025,.F.);
#11680=ORIENTED_EDGE('',*,*,#8222,.T.);
#11681=ORIENTED_EDGE('',*,*,#8183,.F.);
#11682=ORIENTED_EDGE('',*,*,#8033,.F.);
#11683=ORIENTED_EDGE('',*,*,#8061,.F.);
#11684=ORIENTED_EDGE('',*,*,#8223,.T.);
#11685=ORIENTED_EDGE('',*,*,#8039,.T.);
#11686=ORIENTED_EDGE('',*,*,#8224,.F.);
#11687=ORIENTED_EDGE('',*,*,#8064,.F.);
#11688=ORIENTED_EDGE('',*,*,#8224,.T.);
#11689=ORIENTED_EDGE('',*,*,#8038,.T.);
#11690=ORIENTED_EDGE('',*,*,#8225,.F.);
#11691=ORIENTED_EDGE('',*,*,#8066,.F.);
#11692=ORIENTED_EDGE('',*,*,#8225,.T.);
#11693=ORIENTED_EDGE('',*,*,#8037,.T.);
#11694=ORIENTED_EDGE('',*,*,#8071,.F.);
#11695=ORIENTED_EDGE('',*,*,#8058,.F.);
#11696=ORIENTED_EDGE('',*,*,#8068,.T.);
#11697=ORIENTED_EDGE('',*,*,#8040,.T.);
#11698=ORIENTED_EDGE('',*,*,#8223,.F.);
#11699=ORIENTED_EDGE('',*,*,#8226,.T.);
#11700=ORIENTED_EDGE('',*,*,#8227,.T.);
#11701=ORIENTED_EDGE('',*,*,#8228,.T.);
#11702=ORIENTED_EDGE('',*,*,#8229,.T.);
#11703=ORIENTED_EDGE('',*,*,#8230,.T.);
#11704=ORIENTED_EDGE('',*,*,#8231,.T.);
#11705=ORIENTED_EDGE('',*,*,#8232,.T.);
#11706=ORIENTED_EDGE('',*,*,#8233,.T.);
#11707=ORIENTED_EDGE('',*,*,#8226,.F.);
#11708=ORIENTED_EDGE('',*,*,#8234,.T.);
#11709=ORIENTED_EDGE('',*,*,#8235,.T.);
#11710=ORIENTED_EDGE('',*,*,#8236,.T.);
#11711=ORIENTED_EDGE('',*,*,#8232,.F.);
#11712=ORIENTED_EDGE('',*,*,#8237,.T.);
#11713=ORIENTED_EDGE('',*,*,#8238,.T.);
#11714=ORIENTED_EDGE('',*,*,#8239,.T.);
#11715=ORIENTED_EDGE('',*,*,#8235,.F.);
#11716=ORIENTED_EDGE('',*,*,#8240,.T.);
#11717=ORIENTED_EDGE('',*,*,#8241,.T.);
#11718=ORIENTED_EDGE('',*,*,#8242,.T.);
#11719=ORIENTED_EDGE('',*,*,#8238,.F.);
#11720=ORIENTED_EDGE('',*,*,#8243,.T.);
#11721=ORIENTED_EDGE('',*,*,#8244,.T.);
#11722=ORIENTED_EDGE('',*,*,#8245,.T.);
#11723=ORIENTED_EDGE('',*,*,#8241,.F.);
#11724=ORIENTED_EDGE('',*,*,#8246,.T.);
#11725=ORIENTED_EDGE('',*,*,#8247,.T.);
#11726=ORIENTED_EDGE('',*,*,#8248,.T.);
#11727=ORIENTED_EDGE('',*,*,#8244,.F.);
#11728=ORIENTED_EDGE('',*,*,#8249,.T.);
#11729=ORIENTED_EDGE('',*,*,#8230,.F.);
#11730=ORIENTED_EDGE('',*,*,#8250,.T.);
#11731=ORIENTED_EDGE('',*,*,#8247,.F.);
#11732=ORIENTED_EDGE('',*,*,#8251,.T.);
#11733=ORIENTED_EDGE('',*,*,#8227,.F.);
#11734=ORIENTED_EDGE('',*,*,#8233,.F.);
#11735=ORIENTED_EDGE('',*,*,#8236,.F.);
#11736=ORIENTED_EDGE('',*,*,#8239,.F.);
#11737=ORIENTED_EDGE('',*,*,#8242,.F.);
#11738=ORIENTED_EDGE('',*,*,#8245,.F.);
#11739=ORIENTED_EDGE('',*,*,#8248,.F.);
#11740=ORIENTED_EDGE('',*,*,#8250,.F.);
#11741=ORIENTED_EDGE('',*,*,#8229,.F.);
#11742=ORIENTED_EDGE('',*,*,#8252,.F.);
#11743=ORIENTED_EDGE('',*,*,#8253,.T.);
#11744=ORIENTED_EDGE('',*,*,#8254,.F.);
#11745=ORIENTED_EDGE('',*,*,#8255,.F.);
#11746=ORIENTED_EDGE('',*,*,#8256,.F.);
#11747=ORIENTED_EDGE('',*,*,#8257,.F.);
#11748=ORIENTED_EDGE('',*,*,#8258,.F.);
#11749=ORIENTED_EDGE('',*,*,#8259,.F.);
#11750=ORIENTED_EDGE('',*,*,#8260,.F.);
#11751=ORIENTED_EDGE('',*,*,#8261,.F.);
#11752=ORIENTED_EDGE('',*,*,#8262,.F.);
#11753=ORIENTED_EDGE('',*,*,#8263,.T.);
#11754=ORIENTED_EDGE('',*,*,#8264,.F.);
#11755=ORIENTED_EDGE('',*,*,#8240,.F.);
#11756=ORIENTED_EDGE('',*,*,#8265,.T.);
#11757=ORIENTED_EDGE('',*,*,#8266,.T.);
#11758=ORIENTED_EDGE('',*,*,#8267,.F.);
#11759=ORIENTED_EDGE('',*,*,#8237,.F.);
#11760=ORIENTED_EDGE('',*,*,#8268,.T.);
#11761=ORIENTED_EDGE('',*,*,#8269,.T.);
#11762=ORIENTED_EDGE('',*,*,#8265,.F.);
#11763=ORIENTED_EDGE('',*,*,#8234,.F.);
#11764=ORIENTED_EDGE('',*,*,#8270,.T.);
#11765=ORIENTED_EDGE('',*,*,#8271,.T.);
#11766=ORIENTED_EDGE('',*,*,#8268,.F.);
#11767=ORIENTED_EDGE('',*,*,#8231,.F.);
#11768=ORIENTED_EDGE('',*,*,#8272,.T.);
#11769=ORIENTED_EDGE('',*,*,#8273,.T.);
#11770=ORIENTED_EDGE('',*,*,#8270,.F.);
#11771=ORIENTED_EDGE('',*,*,#8274,.F.);
#11772=ORIENTED_EDGE('',*,*,#8275,.F.);
#11773=ORIENTED_EDGE('',*,*,#8276,.F.);
#11774=ORIENTED_EDGE('',*,*,#8277,.T.);
#11775=ORIENTED_EDGE('',*,*,#8278,.T.);
#11776=ORIENTED_EDGE('',*,*,#8275,.T.);
#11777=ORIENTED_EDGE('',*,*,#8279,.T.);
#11778=ORIENTED_EDGE('',*,*,#8280,.T.);
#11779=ORIENTED_EDGE('',*,*,#8281,.T.);
#11780=ORIENTED_EDGE('',*,*,#8282,.T.);
#11781=ORIENTED_EDGE('',*,*,#8276,.T.);
#11782=ORIENTED_EDGE('',*,*,#8283,.T.);
#11783=ORIENTED_EDGE('',*,*,#8284,.T.);
#11784=ORIENTED_EDGE('',*,*,#8252,.T.);
#11785=ORIENTED_EDGE('',*,*,#8285,.T.);
#11786=ORIENTED_EDGE('',*,*,#8274,.T.);
#11787=ORIENTED_EDGE('',*,*,#8286,.T.);
#11788=ORIENTED_EDGE('',*,*,#8283,.F.);
#11789=ORIENTED_EDGE('',*,*,#8278,.F.);
#11790=ORIENTED_EDGE('',*,*,#8287,.F.);
#11791=ORIENTED_EDGE('',*,*,#8288,.F.);
#11792=ORIENTED_EDGE('',*,*,#8277,.F.);
#11793=ORIENTED_EDGE('',*,*,#8289,.F.);
#11794=ORIENTED_EDGE('',*,*,#8290,.T.);
#11795=ORIENTED_EDGE('',*,*,#8291,.T.);
#11796=ORIENTED_EDGE('',*,*,#8287,.T.);
#11797=ORIENTED_EDGE('',*,*,#8280,.F.);
#11798=ORIENTED_EDGE('',*,*,#8292,.T.);
#11799=ORIENTED_EDGE('',*,*,#8264,.T.);
#11800=ORIENTED_EDGE('',*,*,#8293,.T.);
#11801=ORIENTED_EDGE('',*,*,#8289,.T.);
#11802=ORIENTED_EDGE('',*,*,#8279,.F.);
#11803=ORIENTED_EDGE('',*,*,#8285,.F.);
#11804=ORIENTED_EDGE('',*,*,#8228,.F.);
#11805=ORIENTED_EDGE('',*,*,#8292,.F.);
#11806=ORIENTED_EDGE('',*,*,#8294,.T.);
#11807=ORIENTED_EDGE('',*,*,#8295,.F.);
#11808=ORIENTED_EDGE('',*,*,#8296,.T.);
#11809=ORIENTED_EDGE('',*,*,#8297,.T.);
#11810=ORIENTED_EDGE('',*,*,#8298,.T.);
#11811=ORIENTED_EDGE('',*,*,#8299,.F.);
#11812=ORIENTED_EDGE('',*,*,#8300,.T.);
#11813=ORIENTED_EDGE('',*,*,#8301,.T.);
#11814=ORIENTED_EDGE('',*,*,#8299,.T.);
#11815=ORIENTED_EDGE('',*,*,#8302,.T.);
#11816=ORIENTED_EDGE('',*,*,#8303,.T.);
#11817=ORIENTED_EDGE('',*,*,#8304,.T.);
#11818=ORIENTED_EDGE('',*,*,#8305,.T.);
#11819=ORIENTED_EDGE('',*,*,#8306,.T.);
#11820=ORIENTED_EDGE('',*,*,#8307,.T.);
#11821=ORIENTED_EDGE('',*,*,#8308,.T.);
#11822=ORIENTED_EDGE('',*,*,#8305,.F.);
#11823=ORIENTED_EDGE('',*,*,#8309,.T.);
#11824=ORIENTED_EDGE('',*,*,#8303,.F.);
#11825=ORIENTED_EDGE('',*,*,#8310,.T.);
#11826=ORIENTED_EDGE('',*,*,#8295,.T.);
#11827=ORIENTED_EDGE('',*,*,#8311,.T.);
#11828=ORIENTED_EDGE('',*,*,#8312,.T.);
#11829=ORIENTED_EDGE('',*,*,#8313,.T.);
#11830=ORIENTED_EDGE('',*,*,#8312,.F.);
#11831=ORIENTED_EDGE('',*,*,#8314,.T.);
#11832=ORIENTED_EDGE('',*,*,#8307,.F.);
#11833=ORIENTED_EDGE('',*,*,#8315,.T.);
#11834=ORIENTED_EDGE('',*,*,#8311,.F.);
#11835=ORIENTED_EDGE('',*,*,#8294,.F.);
#11836=ORIENTED_EDGE('',*,*,#8316,.T.);
#11837=ORIENTED_EDGE('',*,*,#8317,.F.);
#11838=ORIENTED_EDGE('',*,*,#8318,.F.);
#11839=ORIENTED_EDGE('',*,*,#8319,.T.);
#11840=ORIENTED_EDGE('',*,*,#8297,.F.);
#11841=ORIENTED_EDGE('',*,*,#8320,.T.);
#11842=ORIENTED_EDGE('',*,*,#8321,.F.);
#11843=ORIENTED_EDGE('',*,*,#8322,.F.);
#11844=ORIENTED_EDGE('',*,*,#8323,.F.);
#11845=ORIENTED_EDGE('',*,*,#8316,.F.);
#11846=ORIENTED_EDGE('',*,*,#8296,.F.);
#11847=ORIENTED_EDGE('',*,*,#8313,.F.);
#11848=ORIENTED_EDGE('',*,*,#8315,.F.);
#11849=ORIENTED_EDGE('',*,*,#8306,.F.);
#11850=ORIENTED_EDGE('',*,*,#8310,.F.);
#11851=ORIENTED_EDGE('',*,*,#8302,.F.);
#11852=ORIENTED_EDGE('',*,*,#8298,.F.);
#11853=ORIENTED_EDGE('',*,*,#8324,.T.);
#11854=ORIENTED_EDGE('',*,*,#8325,.F.);
#11855=ORIENTED_EDGE('',*,*,#8320,.F.);
#11856=ORIENTED_EDGE('',*,*,#8326,.T.);
#11857=ORIENTED_EDGE('',*,*,#8327,.F.);
#11858=ORIENTED_EDGE('',*,*,#8328,.T.);
#11859=ORIENTED_EDGE('',*,*,#8329,.T.);
#11860=ORIENTED_EDGE('',*,*,#8330,.T.);
#11861=ORIENTED_EDGE('',*,*,#8331,.F.);
#11862=ORIENTED_EDGE('',*,*,#8317,.T.);
#11863=ORIENTED_EDGE('',*,*,#8323,.T.);
#11864=ORIENTED_EDGE('',*,*,#8331,.T.);
#11865=ORIENTED_EDGE('',*,*,#8332,.T.);
#11866=ORIENTED_EDGE('',*,*,#8333,.T.);
#11867=ORIENTED_EDGE('',*,*,#8318,.T.);
#11868=ORIENTED_EDGE('',*,*,#8334,.T.);
#11869=ORIENTED_EDGE('',*,*,#8335,.T.);
#11870=ORIENTED_EDGE('',*,*,#8336,.T.);
#11871=ORIENTED_EDGE('',*,*,#8337,.T.);
#11872=ORIENTED_EDGE('',*,*,#8334,.F.);
#11873=ORIENTED_EDGE('',*,*,#8338,.T.);
#11874=ORIENTED_EDGE('',*,*,#8333,.F.);
#11875=ORIENTED_EDGE('',*,*,#8339,.T.);
#11876=ORIENTED_EDGE('',*,*,#8327,.T.);
#11877=ORIENTED_EDGE('',*,*,#8340,.T.);
#11878=ORIENTED_EDGE('',*,*,#8341,.T.);
#11879=ORIENTED_EDGE('',*,*,#8342,.T.);
#11880=ORIENTED_EDGE('',*,*,#8341,.F.);
#11881=ORIENTED_EDGE('',*,*,#8343,.T.);
#11882=ORIENTED_EDGE('',*,*,#8336,.F.);
#11883=ORIENTED_EDGE('',*,*,#8344,.T.);
#11884=ORIENTED_EDGE('',*,*,#8314,.F.);
#11885=ORIENTED_EDGE('',*,*,#8319,.F.);
#11886=ORIENTED_EDGE('',*,*,#8338,.F.);
#11887=ORIENTED_EDGE('',*,*,#8337,.F.);
#11888=ORIENTED_EDGE('',*,*,#8343,.F.);
#11889=ORIENTED_EDGE('',*,*,#8345,.F.);
#11890=ORIENTED_EDGE('',*,*,#8346,.F.);
#11891=ORIENTED_EDGE('',*,*,#8347,.F.);
#11892=ORIENTED_EDGE('',*,*,#8348,.F.);
#11893=ORIENTED_EDGE('',*,*,#8349,.F.);
#11894=ORIENTED_EDGE('',*,*,#8350,.F.);
#11895=ORIENTED_EDGE('',*,*,#8351,.F.);
#11896=ORIENTED_EDGE('',*,*,#8352,.F.);
#11897=ORIENTED_EDGE('',*,*,#8353,.F.);
#11898=ORIENTED_EDGE('',*,*,#8309,.F.);
#11899=ORIENTED_EDGE('',*,*,#8308,.F.);
#11900=ORIENTED_EDGE('',*,*,#8354,.F.);
#11901=ORIENTED_EDGE('',*,*,#8291,.F.);
#11902=ORIENTED_EDGE('',*,*,#8355,.F.);
#11903=ORIENTED_EDGE('',*,*,#8284,.F.);
#11904=ORIENTED_EDGE('',*,*,#8288,.T.);
#11905=ORIENTED_EDGE('',*,*,#8354,.T.);
#11906=ORIENTED_EDGE('',*,*,#8356,.T.);
#11907=ORIENTED_EDGE('',*,*,#8357,.T.);
#11908=ORIENTED_EDGE('',*,*,#8358,.T.);
#11909=ORIENTED_EDGE('',*,*,#8359,.T.);
#11910=ORIENTED_EDGE('',*,*,#8254,.T.);
#11911=ORIENTED_EDGE('',*,*,#8360,.T.);
#11912=ORIENTED_EDGE('',*,*,#8361,.T.);
#11913=ORIENTED_EDGE('',*,*,#8255,.T.);
#11914=ORIENTED_EDGE('',*,*,#8359,.F.);
#11915=ORIENTED_EDGE('',*,*,#8362,.T.);
#11916=ORIENTED_EDGE('',*,*,#8363,.T.);
#11917=ORIENTED_EDGE('',*,*,#8256,.T.);
#11918=ORIENTED_EDGE('',*,*,#8361,.F.);
#11919=ORIENTED_EDGE('',*,*,#8364,.T.);
#11920=ORIENTED_EDGE('',*,*,#8365,.T.);
#11921=ORIENTED_EDGE('',*,*,#8257,.T.);
#11922=ORIENTED_EDGE('',*,*,#8363,.F.);
#11923=ORIENTED_EDGE('',*,*,#8366,.T.);
#11924=ORIENTED_EDGE('',*,*,#8367,.T.);
#11925=ORIENTED_EDGE('',*,*,#8258,.T.);
#11926=ORIENTED_EDGE('',*,*,#8365,.F.);
#11927=ORIENTED_EDGE('',*,*,#8321,.T.);
#11928=ORIENTED_EDGE('',*,*,#8368,.T.);
#11929=ORIENTED_EDGE('',*,*,#8259,.T.);
#11930=ORIENTED_EDGE('',*,*,#8367,.F.);
#11931=ORIENTED_EDGE('',*,*,#8325,.T.);
#11932=ORIENTED_EDGE('',*,*,#8369,.T.);
#11933=ORIENTED_EDGE('',*,*,#8260,.T.);
#11934=ORIENTED_EDGE('',*,*,#8368,.F.);
#11935=ORIENTED_EDGE('',*,*,#8370,.T.);
#11936=ORIENTED_EDGE('',*,*,#8371,.T.);
#11937=ORIENTED_EDGE('',*,*,#8261,.T.);
#11938=ORIENTED_EDGE('',*,*,#8369,.F.);
#11939=ORIENTED_EDGE('',*,*,#8372,.T.);
#11940=ORIENTED_EDGE('',*,*,#8262,.T.);
#11941=ORIENTED_EDGE('',*,*,#8371,.F.);
#11942=ORIENTED_EDGE('',*,*,#8373,.T.);
#11943=ORIENTED_EDGE('',*,*,#8374,.T.);
#11944=ORIENTED_EDGE('',*,*,#8281,.F.);
#11945=ORIENTED_EDGE('',*,*,#8357,.F.);
#11946=ORIENTED_EDGE('',*,*,#8375,.T.);
#11947=ORIENTED_EDGE('',*,*,#8360,.F.);
#11948=ORIENTED_EDGE('',*,*,#8376,.T.);
#11949=ORIENTED_EDGE('',*,*,#8377,.T.);
#11950=ORIENTED_EDGE('',*,*,#8355,.T.);
#11951=ORIENTED_EDGE('',*,*,#8378,.T.);
#11952=ORIENTED_EDGE('',*,*,#8374,.F.);
#11953=ORIENTED_EDGE('',*,*,#8330,.F.);
#11954=ORIENTED_EDGE('',*,*,#8322,.T.);
#11955=ORIENTED_EDGE('',*,*,#8366,.F.);
#11956=ORIENTED_EDGE('',*,*,#8379,.F.);
#11957=ORIENTED_EDGE('',*,*,#8328,.F.);
#11958=ORIENTED_EDGE('',*,*,#8342,.F.);
#11959=ORIENTED_EDGE('',*,*,#8344,.F.);
#11960=ORIENTED_EDGE('',*,*,#8335,.F.);
#11961=ORIENTED_EDGE('',*,*,#8339,.F.);
#11962=ORIENTED_EDGE('',*,*,#8332,.F.);
#11963=ORIENTED_EDGE('',*,*,#8329,.F.);
#11964=ORIENTED_EDGE('',*,*,#8379,.T.);
#11965=ORIENTED_EDGE('',*,*,#8364,.F.);
#11966=ORIENTED_EDGE('',*,*,#8380,.F.);
#11967=ORIENTED_EDGE('',*,*,#8381,.F.);
#11968=ORIENTED_EDGE('',*,*,#8382,.F.);
#11969=ORIENTED_EDGE('',*,*,#8362,.F.);
#11970=ORIENTED_EDGE('',*,*,#8383,.F.);
#11971=ORIENTED_EDGE('',*,*,#8384,.F.);
#11972=ORIENTED_EDGE('',*,*,#8385,.F.);
#11973=ORIENTED_EDGE('',*,*,#8386,.F.);
#11974=ORIENTED_EDGE('',*,*,#8387,.F.);
#11975=ORIENTED_EDGE('',*,*,#8388,.F.);
#11976=ORIENTED_EDGE('',*,*,#8389,.F.);
#11977=ORIENTED_EDGE('',*,*,#8390,.F.);
#11978=ORIENTED_EDGE('',*,*,#8380,.T.);
#11979=ORIENTED_EDGE('',*,*,#8293,.F.);
#11980=ORIENTED_EDGE('',*,*,#8263,.F.);
#11981=ORIENTED_EDGE('',*,*,#8378,.F.);
#11982=ORIENTED_EDGE('',*,*,#8290,.F.);
#11983=ORIENTED_EDGE('',*,*,#8282,.F.);
#11984=ORIENTED_EDGE('',*,*,#8376,.F.);
#11985=ORIENTED_EDGE('',*,*,#8253,.F.);
#11986=ORIENTED_EDGE('',*,*,#8286,.F.);
#11987=ORIENTED_EDGE('',*,*,#8391,.T.);
#11988=ORIENTED_EDGE('',*,*,#8392,.F.);
#11989=ORIENTED_EDGE('',*,*,#8393,.T.);
#11990=ORIENTED_EDGE('',*,*,#8394,.T.);
#11991=ORIENTED_EDGE('',*,*,#8395,.T.);
#11992=ORIENTED_EDGE('',*,*,#8396,.F.);
#11993=ORIENTED_EDGE('',*,*,#8397,.T.);
#11994=ORIENTED_EDGE('',*,*,#8398,.T.);
#11995=ORIENTED_EDGE('',*,*,#8396,.T.);
#11996=ORIENTED_EDGE('',*,*,#8399,.T.);
#11997=ORIENTED_EDGE('',*,*,#8400,.T.);
#11998=ORIENTED_EDGE('',*,*,#8401,.T.);
#11999=ORIENTED_EDGE('',*,*,#8402,.T.);
#12000=ORIENTED_EDGE('',*,*,#8403,.T.);
#12001=ORIENTED_EDGE('',*,*,#8404,.T.);
#12002=ORIENTED_EDGE('',*,*,#8351,.T.);
#12003=ORIENTED_EDGE('',*,*,#8402,.F.);
#12004=ORIENTED_EDGE('',*,*,#8350,.T.);
#12005=ORIENTED_EDGE('',*,*,#8400,.F.);
#12006=ORIENTED_EDGE('',*,*,#8405,.T.);
#12007=ORIENTED_EDGE('',*,*,#8392,.T.);
#12008=ORIENTED_EDGE('',*,*,#8406,.T.);
#12009=ORIENTED_EDGE('',*,*,#8407,.T.);
#12010=ORIENTED_EDGE('',*,*,#8408,.T.);
#12011=ORIENTED_EDGE('',*,*,#8407,.F.);
#12012=ORIENTED_EDGE('',*,*,#8352,.T.);
#12013=ORIENTED_EDGE('',*,*,#8404,.F.);
#12014=ORIENTED_EDGE('',*,*,#8409,.T.);
#12015=ORIENTED_EDGE('',*,*,#8304,.F.);
#12016=ORIENTED_EDGE('',*,*,#8353,.T.);
#12017=ORIENTED_EDGE('',*,*,#8406,.F.);
#12018=ORIENTED_EDGE('',*,*,#8391,.F.);
#12019=ORIENTED_EDGE('',*,*,#8410,.T.);
#12020=ORIENTED_EDGE('',*,*,#8300,.F.);
#12021=ORIENTED_EDGE('',*,*,#8301,.F.);
#12022=ORIENTED_EDGE('',*,*,#8410,.F.);
#12023=ORIENTED_EDGE('',*,*,#8394,.F.);
#12024=ORIENTED_EDGE('',*,*,#8411,.T.);
#12025=ORIENTED_EDGE('',*,*,#8370,.F.);
#12026=ORIENTED_EDGE('',*,*,#8324,.F.);
#12027=ORIENTED_EDGE('',*,*,#8372,.F.);
#12028=ORIENTED_EDGE('',*,*,#8411,.F.);
#12029=ORIENTED_EDGE('',*,*,#8393,.F.);
#12030=ORIENTED_EDGE('',*,*,#8408,.F.);
#12031=ORIENTED_EDGE('',*,*,#8409,.F.);
#12032=ORIENTED_EDGE('',*,*,#8403,.F.);
#12033=ORIENTED_EDGE('',*,*,#8405,.F.);
#12034=ORIENTED_EDGE('',*,*,#8399,.F.);
#12035=ORIENTED_EDGE('',*,*,#8395,.F.);
#12036=ORIENTED_EDGE('',*,*,#8412,.T.);
#12037=ORIENTED_EDGE('',*,*,#8413,.T.);
#12038=ORIENTED_EDGE('',*,*,#8414,.F.);
#12039=ORIENTED_EDGE('',*,*,#8384,.T.);
#12040=ORIENTED_EDGE('',*,*,#8415,.T.);
#12041=ORIENTED_EDGE('',*,*,#8390,.T.);
#12042=ORIENTED_EDGE('',*,*,#8416,.F.);
#12043=ORIENTED_EDGE('',*,*,#8417,.T.);
#12044=ORIENTED_EDGE('',*,*,#8381,.T.);
#12045=ORIENTED_EDGE('',*,*,#8416,.T.);
#12046=ORIENTED_EDGE('',*,*,#8389,.T.);
#12047=ORIENTED_EDGE('',*,*,#8418,.T.);
#12048=ORIENTED_EDGE('',*,*,#8419,.T.);
#12049=ORIENTED_EDGE('',*,*,#8420,.T.);
#12050=ORIENTED_EDGE('',*,*,#8387,.T.);
#12051=ORIENTED_EDGE('',*,*,#8421,.T.);
#12052=ORIENTED_EDGE('',*,*,#8347,.T.);
#12053=ORIENTED_EDGE('',*,*,#8420,.F.);
#12054=ORIENTED_EDGE('',*,*,#8346,.T.);
#12055=ORIENTED_EDGE('',*,*,#8418,.F.);
#12056=ORIENTED_EDGE('',*,*,#8388,.T.);
#12057=ORIENTED_EDGE('',*,*,#8414,.T.);
#12058=ORIENTED_EDGE('',*,*,#8422,.T.);
#12059=ORIENTED_EDGE('',*,*,#8423,.T.);
#12060=ORIENTED_EDGE('',*,*,#8385,.T.);
#12061=ORIENTED_EDGE('',*,*,#8423,.F.);
#12062=ORIENTED_EDGE('',*,*,#8348,.T.);
#12063=ORIENTED_EDGE('',*,*,#8421,.F.);
#12064=ORIENTED_EDGE('',*,*,#8386,.T.);
#12065=ORIENTED_EDGE('',*,*,#8326,.F.);
#12066=ORIENTED_EDGE('',*,*,#8382,.T.);
#12067=ORIENTED_EDGE('',*,*,#8417,.F.);
#12068=ORIENTED_EDGE('',*,*,#8419,.F.);
#12069=ORIENTED_EDGE('',*,*,#8345,.T.);
#12070=ORIENTED_EDGE('',*,*,#8340,.F.);
#12071=ORIENTED_EDGE('',*,*,#8401,.F.);
#12072=ORIENTED_EDGE('',*,*,#8349,.T.);
#12073=ORIENTED_EDGE('',*,*,#8422,.F.);
#12074=ORIENTED_EDGE('',*,*,#8413,.F.);
#12075=ORIENTED_EDGE('',*,*,#8424,.T.);
#12076=ORIENTED_EDGE('',*,*,#8397,.F.);
#12077=ORIENTED_EDGE('',*,*,#8373,.F.);
#12078=ORIENTED_EDGE('',*,*,#8412,.F.);
#12079=ORIENTED_EDGE('',*,*,#8398,.F.);
#12080=ORIENTED_EDGE('',*,*,#8424,.F.);
#12081=ORIENTED_EDGE('',*,*,#8415,.F.);
#12082=ORIENTED_EDGE('',*,*,#8383,.T.);
#12083=ORIENTED_EDGE('',*,*,#8358,.F.);
#12084=ORIENTED_EDGE('',*,*,#8375,.F.);
#12085=ORIENTED_EDGE('',*,*,#8356,.F.);
#12086=ORIENTED_EDGE('',*,*,#8377,.F.);
#12087=ORIENTED_EDGE('',*,*,#8251,.F.);
#12088=ORIENTED_EDGE('',*,*,#8425,.T.);
#12089=ORIENTED_EDGE('',*,*,#8426,.T.);
#12090=ORIENTED_EDGE('',*,*,#8272,.F.);
#12091=ORIENTED_EDGE('',*,*,#8249,.F.);
#12092=ORIENTED_EDGE('',*,*,#8427,.T.);
#12093=ORIENTED_EDGE('',*,*,#8428,.T.);
#12094=ORIENTED_EDGE('',*,*,#8425,.F.);
#12095=ORIENTED_EDGE('',*,*,#8246,.F.);
#12096=ORIENTED_EDGE('',*,*,#8429,.T.);
#12097=ORIENTED_EDGE('',*,*,#8430,.T.);
#12098=ORIENTED_EDGE('',*,*,#8427,.F.);
#12099=ORIENTED_EDGE('',*,*,#8243,.F.);
#12100=ORIENTED_EDGE('',*,*,#8267,.T.);
#12101=ORIENTED_EDGE('',*,*,#8431,.T.);
#12102=ORIENTED_EDGE('',*,*,#8429,.F.);
#12103=ORIENTED_EDGE('',*,*,#8271,.F.);
#12104=ORIENTED_EDGE('',*,*,#8273,.F.);
#12105=ORIENTED_EDGE('',*,*,#8426,.F.);
#12106=ORIENTED_EDGE('',*,*,#8428,.F.);
#12107=ORIENTED_EDGE('',*,*,#8430,.F.);
#12108=ORIENTED_EDGE('',*,*,#8431,.F.);
#12109=ORIENTED_EDGE('',*,*,#8266,.F.);
#12110=ORIENTED_EDGE('',*,*,#8269,.F.);
#12111=ORIENTED_EDGE('',*,*,#8432,.T.);
#12112=ORIENTED_EDGE('',*,*,#8433,.T.);
#12113=ORIENTED_EDGE('',*,*,#8434,.T.);
#12114=ORIENTED_EDGE('',*,*,#8433,.F.);
#12115=ORIENTED_EDGE('',*,*,#8435,.F.);
#12116=ORIENTED_EDGE('',*,*,#8436,.T.);
#12117=ORIENTED_EDGE('',*,*,#8432,.F.);
#12118=ORIENTED_EDGE('',*,*,#8436,.F.);
#12119=ORIENTED_EDGE('',*,*,#8437,.F.);
#12120=ORIENTED_EDGE('',*,*,#8438,.F.);
#12121=ORIENTED_EDGE('',*,*,#8439,.F.);
#12122=ORIENTED_EDGE('',*,*,#8440,.F.);
#12123=ORIENTED_EDGE('',*,*,#8441,.F.);
#12124=ORIENTED_EDGE('',*,*,#8442,.F.);
#12125=ORIENTED_EDGE('',*,*,#8443,.F.);
#12126=ORIENTED_EDGE('',*,*,#8444,.F.);
#12127=ORIENTED_EDGE('',*,*,#8445,.F.);
#12128=ORIENTED_EDGE('',*,*,#8446,.F.);
#12129=ORIENTED_EDGE('',*,*,#8434,.F.);
#12130=ORIENTED_EDGE('',*,*,#8447,.T.);
#12131=ORIENTED_EDGE('',*,*,#8448,.T.);
#12132=ORIENTED_EDGE('',*,*,#8435,.T.);
#12133=ORIENTED_EDGE('',*,*,#8448,.F.);
#12134=ORIENTED_EDGE('',*,*,#8449,.T.);
#12135=ORIENTED_EDGE('',*,*,#8450,.T.);
#12136=ORIENTED_EDGE('',*,*,#8451,.F.);
#12137=ORIENTED_EDGE('',*,*,#8452,.T.);
#12138=ORIENTED_EDGE('',*,*,#8453,.T.);
#12139=ORIENTED_EDGE('',*,*,#8454,.F.);
#12140=ORIENTED_EDGE('',*,*,#8455,.T.);
#12141=ORIENTED_EDGE('',*,*,#8456,.T.);
#12142=ORIENTED_EDGE('',*,*,#8457,.F.);
#12143=ORIENTED_EDGE('',*,*,#8458,.T.);
#12144=ORIENTED_EDGE('',*,*,#8459,.T.);
#12145=ORIENTED_EDGE('',*,*,#8460,.F.);
#12146=ORIENTED_EDGE('',*,*,#8461,.T.);
#12147=ORIENTED_EDGE('',*,*,#8462,.T.);
#12148=ORIENTED_EDGE('',*,*,#8463,.F.);
#12149=ORIENTED_EDGE('',*,*,#8464,.T.);
#12150=ORIENTED_EDGE('',*,*,#8465,.T.);
#12151=ORIENTED_EDGE('',*,*,#8466,.F.);
#12152=ORIENTED_EDGE('',*,*,#8467,.T.);
#12153=ORIENTED_EDGE('',*,*,#8468,.T.);
#12154=ORIENTED_EDGE('',*,*,#8469,.F.);
#12155=ORIENTED_EDGE('',*,*,#8470,.T.);
#12156=ORIENTED_EDGE('',*,*,#8471,.T.);
#12157=ORIENTED_EDGE('',*,*,#8472,.F.);
#12158=ORIENTED_EDGE('',*,*,#8473,.T.);
#12159=ORIENTED_EDGE('',*,*,#8474,.T.);
#12160=ORIENTED_EDGE('',*,*,#8475,.F.);
#12161=ORIENTED_EDGE('',*,*,#8476,.T.);
#12162=ORIENTED_EDGE('',*,*,#8477,.T.);
#12163=ORIENTED_EDGE('',*,*,#8478,.F.);
#12164=ORIENTED_EDGE('',*,*,#8479,.T.);
#12165=ORIENTED_EDGE('',*,*,#8480,.T.);
#12166=ORIENTED_EDGE('',*,*,#8481,.F.);
#12167=ORIENTED_EDGE('',*,*,#8482,.T.);
#12168=ORIENTED_EDGE('',*,*,#8483,.T.);
#12169=ORIENTED_EDGE('',*,*,#8484,.F.);
#12170=ORIENTED_EDGE('',*,*,#8485,.T.);
#12171=ORIENTED_EDGE('',*,*,#8486,.T.);
#12172=ORIENTED_EDGE('',*,*,#8487,.F.);
#12173=ORIENTED_EDGE('',*,*,#8488,.T.);
#12174=ORIENTED_EDGE('',*,*,#8489,.T.);
#12175=ORIENTED_EDGE('',*,*,#8490,.F.);
#12176=ORIENTED_EDGE('',*,*,#8491,.T.);
#12177=ORIENTED_EDGE('',*,*,#8492,.T.);
#12178=ORIENTED_EDGE('',*,*,#8493,.F.);
#12179=ORIENTED_EDGE('',*,*,#8494,.T.);
#12180=ORIENTED_EDGE('',*,*,#8495,.T.);
#12181=ORIENTED_EDGE('',*,*,#8496,.F.);
#12182=ORIENTED_EDGE('',*,*,#8497,.T.);
#12183=ORIENTED_EDGE('',*,*,#8498,.T.);
#12184=ORIENTED_EDGE('',*,*,#8499,.F.);
#12185=ORIENTED_EDGE('',*,*,#8500,.T.);
#12186=ORIENTED_EDGE('',*,*,#8501,.T.);
#12187=ORIENTED_EDGE('',*,*,#8502,.F.);
#12188=ORIENTED_EDGE('',*,*,#8503,.T.);
#12189=ORIENTED_EDGE('',*,*,#8504,.T.);
#12190=ORIENTED_EDGE('',*,*,#8505,.F.);
#12191=ORIENTED_EDGE('',*,*,#8506,.T.);
#12192=ORIENTED_EDGE('',*,*,#8507,.T.);
#12193=ORIENTED_EDGE('',*,*,#8508,.F.);
#12194=ORIENTED_EDGE('',*,*,#8447,.F.);
#12195=ORIENTED_EDGE('',*,*,#8509,.T.);
#12196=ORIENTED_EDGE('',*,*,#8510,.T.);
#12197=ORIENTED_EDGE('',*,*,#8511,.T.);
#12198=ORIENTED_EDGE('',*,*,#8508,.T.);
#12199=ORIENTED_EDGE('',*,*,#8510,.F.);
#12200=ORIENTED_EDGE('',*,*,#8512,.F.);
#12201=ORIENTED_EDGE('',*,*,#8513,.T.);
#12202=ORIENTED_EDGE('',*,*,#8514,.T.);
#12203=ORIENTED_EDGE('',*,*,#8515,.T.);
#12204=ORIENTED_EDGE('',*,*,#8516,.T.);
#12205=ORIENTED_EDGE('',*,*,#8517,.T.);
#12206=ORIENTED_EDGE('',*,*,#8454,.T.);
#12207=ORIENTED_EDGE('',*,*,#8516,.F.);
#12208=ORIENTED_EDGE('',*,*,#8518,.F.);
#12209=ORIENTED_EDGE('',*,*,#8519,.T.);
#12210=ORIENTED_EDGE('',*,*,#8520,.T.);
#12211=ORIENTED_EDGE('',*,*,#8521,.T.);
#12212=ORIENTED_EDGE('',*,*,#8522,.T.);
#12213=ORIENTED_EDGE('',*,*,#8523,.T.);
#12214=ORIENTED_EDGE('',*,*,#8460,.T.);
#12215=ORIENTED_EDGE('',*,*,#8522,.F.);
#12216=ORIENTED_EDGE('',*,*,#8524,.F.);
#12217=ORIENTED_EDGE('',*,*,#8525,.T.);
#12218=ORIENTED_EDGE('',*,*,#8526,.T.);
#12219=ORIENTED_EDGE('',*,*,#8527,.F.);
#12220=ORIENTED_EDGE('',*,*,#8528,.F.);
#12221=ORIENTED_EDGE('',*,*,#8529,.F.);
#12222=ORIENTED_EDGE('',*,*,#8530,.T.);
#12223=ORIENTED_EDGE('',*,*,#8437,.T.);
#12224=ORIENTED_EDGE('',*,*,#8528,.T.);
#12225=ORIENTED_EDGE('',*,*,#8531,.T.);
#12226=ORIENTED_EDGE('',*,*,#8532,.T.);
#12227=ORIENTED_EDGE('',*,*,#8533,.F.);
#12228=ORIENTED_EDGE('',*,*,#8534,.F.);
#12229=ORIENTED_EDGE('',*,*,#8535,.F.);
#12230=ORIENTED_EDGE('',*,*,#8534,.T.);
#12231=ORIENTED_EDGE('',*,*,#8536,.T.);
#12232=ORIENTED_EDGE('',*,*,#8529,.T.);
#12233=ORIENTED_EDGE('',*,*,#8446,.T.);
#12234=ORIENTED_EDGE('',*,*,#8537,.F.);
#12235=ORIENTED_EDGE('',*,*,#8538,.F.);
#12236=ORIENTED_EDGE('',*,*,#8539,.F.);
#12237=ORIENTED_EDGE('',*,*,#8538,.T.);
#12238=ORIENTED_EDGE('',*,*,#8540,.T.);
#12239=ORIENTED_EDGE('',*,*,#8535,.T.);
#12240=ORIENTED_EDGE('',*,*,#8445,.T.);
#12241=ORIENTED_EDGE('',*,*,#8541,.T.);
#12242=ORIENTED_EDGE('',*,*,#8542,.T.);
#12243=ORIENTED_EDGE('',*,*,#8539,.T.);
#12244=ORIENTED_EDGE('',*,*,#8444,.T.);
#12245=ORIENTED_EDGE('',*,*,#8543,.T.);
#12246=ORIENTED_EDGE('',*,*,#8463,.T.);
#12247=ORIENTED_EDGE('',*,*,#8544,.T.);
#12248=ORIENTED_EDGE('',*,*,#8537,.T.);
#12249=ORIENTED_EDGE('',*,*,#8545,.T.);
#12250=ORIENTED_EDGE('',*,*,#8457,.T.);
#12251=ORIENTED_EDGE('',*,*,#8546,.T.);
#12252=ORIENTED_EDGE('',*,*,#8533,.T.);
#12253=ORIENTED_EDGE('',*,*,#8547,.T.);
#12254=ORIENTED_EDGE('',*,*,#8451,.T.);
#12255=ORIENTED_EDGE('',*,*,#8548,.T.);
#12256=ORIENTED_EDGE('',*,*,#8527,.T.);
#12257=ORIENTED_EDGE('',*,*,#8549,.T.);
#12258=ORIENTED_EDGE('',*,*,#8549,.F.);
#12259=ORIENTED_EDGE('',*,*,#8536,.F.);
#12260=ORIENTED_EDGE('',*,*,#8546,.F.);
#12261=ORIENTED_EDGE('',*,*,#8456,.F.);
#12262=ORIENTED_EDGE('',*,*,#8550,.T.);
#12263=ORIENTED_EDGE('',*,*,#8551,.T.);
#12264=ORIENTED_EDGE('',*,*,#8552,.T.);
#12265=ORIENTED_EDGE('',*,*,#8452,.F.);
#12266=ORIENTED_EDGE('',*,*,#8547,.F.);
#12267=ORIENTED_EDGE('',*,*,#8540,.F.);
#12268=ORIENTED_EDGE('',*,*,#8544,.F.);
#12269=ORIENTED_EDGE('',*,*,#8462,.F.);
#12270=ORIENTED_EDGE('',*,*,#8553,.T.);
#12271=ORIENTED_EDGE('',*,*,#8554,.T.);
#12272=ORIENTED_EDGE('',*,*,#8555,.T.);
#12273=ORIENTED_EDGE('',*,*,#8458,.F.);
#12274=ORIENTED_EDGE('',*,*,#8545,.F.);
#12275=ORIENTED_EDGE('',*,*,#8542,.F.);
#12276=ORIENTED_EDGE('',*,*,#8556,.F.);
#12277=ORIENTED_EDGE('',*,*,#8468,.F.);
#12278=ORIENTED_EDGE('',*,*,#8557,.T.);
#12279=ORIENTED_EDGE('',*,*,#8558,.T.);
#12280=ORIENTED_EDGE('',*,*,#8559,.T.);
#12281=ORIENTED_EDGE('',*,*,#8464,.F.);
#12282=ORIENTED_EDGE('',*,*,#8541,.F.);
#12283=ORIENTED_EDGE('',*,*,#8560,.F.);
#12284=ORIENTED_EDGE('',*,*,#8561,.T.);
#12285=ORIENTED_EDGE('',*,*,#8469,.T.);
#12286=ORIENTED_EDGE('',*,*,#8556,.T.);
#12287=ORIENTED_EDGE('',*,*,#8543,.F.);
#12288=ORIENTED_EDGE('',*,*,#8443,.T.);
#12289=ORIENTED_EDGE('',*,*,#8562,.T.);
#12290=ORIENTED_EDGE('',*,*,#8563,.T.);
#12291=ORIENTED_EDGE('',*,*,#8560,.T.);
#12292=ORIENTED_EDGE('',*,*,#8564,.T.);
#12293=ORIENTED_EDGE('',*,*,#8565,.T.);
#12294=ORIENTED_EDGE('',*,*,#8566,.T.);
#12295=ORIENTED_EDGE('',*,*,#8466,.T.);
#12296=ORIENTED_EDGE('',*,*,#8565,.F.);
#12297=ORIENTED_EDGE('',*,*,#8567,.F.);
#12298=ORIENTED_EDGE('',*,*,#8568,.T.);
#12299=ORIENTED_EDGE('',*,*,#8569,.T.);
#12300=ORIENTED_EDGE('',*,*,#8570,.T.);
#12301=ORIENTED_EDGE('',*,*,#8571,.T.);
#12302=ORIENTED_EDGE('',*,*,#8572,.T.);
#12303=ORIENTED_EDGE('',*,*,#8472,.T.);
#12304=ORIENTED_EDGE('',*,*,#8571,.F.);
#12305=ORIENTED_EDGE('',*,*,#8573,.F.);
#12306=ORIENTED_EDGE('',*,*,#8574,.T.);
#12307=ORIENTED_EDGE('',*,*,#8575,.T.);
#12308=ORIENTED_EDGE('',*,*,#8576,.T.);
#12309=ORIENTED_EDGE('',*,*,#8577,.T.);
#12310=ORIENTED_EDGE('',*,*,#8578,.T.);
#12311=ORIENTED_EDGE('',*,*,#8478,.T.);
#12312=ORIENTED_EDGE('',*,*,#8577,.F.);
#12313=ORIENTED_EDGE('',*,*,#8579,.F.);
#12314=ORIENTED_EDGE('',*,*,#8580,.T.);
#12315=ORIENTED_EDGE('',*,*,#8581,.T.);
#12316=ORIENTED_EDGE('',*,*,#8582,.T.);
#12317=ORIENTED_EDGE('',*,*,#8583,.T.);
#12318=ORIENTED_EDGE('',*,*,#8584,.T.);
#12319=ORIENTED_EDGE('',*,*,#8484,.T.);
#12320=ORIENTED_EDGE('',*,*,#8583,.F.);
#12321=ORIENTED_EDGE('',*,*,#8585,.F.);
#12322=ORIENTED_EDGE('',*,*,#8586,.T.);
#12323=ORIENTED_EDGE('',*,*,#8587,.T.);
#12324=ORIENTED_EDGE('',*,*,#8588,.T.);
#12325=ORIENTED_EDGE('',*,*,#8589,.T.);
#12326=ORIENTED_EDGE('',*,*,#8590,.T.);
#12327=ORIENTED_EDGE('',*,*,#8490,.T.);
#12328=ORIENTED_EDGE('',*,*,#8589,.F.);
#12329=ORIENTED_EDGE('',*,*,#8591,.F.);
#12330=ORIENTED_EDGE('',*,*,#8592,.T.);
#12331=ORIENTED_EDGE('',*,*,#8593,.T.);
#12332=ORIENTED_EDGE('',*,*,#8594,.T.);
#12333=ORIENTED_EDGE('',*,*,#8595,.T.);
#12334=ORIENTED_EDGE('',*,*,#8596,.T.);
#12335=ORIENTED_EDGE('',*,*,#8496,.T.);
#12336=ORIENTED_EDGE('',*,*,#8595,.F.);
#12337=ORIENTED_EDGE('',*,*,#8597,.F.);
#12338=ORIENTED_EDGE('',*,*,#8598,.T.);
#12339=ORIENTED_EDGE('',*,*,#8599,.T.);
#12340=ORIENTED_EDGE('',*,*,#8600,.F.);
#12341=ORIENTED_EDGE('',*,*,#8562,.F.);
#12342=ORIENTED_EDGE('',*,*,#8601,.F.);
#12343=ORIENTED_EDGE('',*,*,#8602,.F.);
#12344=ORIENTED_EDGE('',*,*,#8603,.F.);
#12345=ORIENTED_EDGE('',*,*,#8604,.F.);
#12346=ORIENTED_EDGE('',*,*,#8603,.T.);
#12347=ORIENTED_EDGE('',*,*,#8605,.T.);
#12348=ORIENTED_EDGE('',*,*,#8601,.T.);
#12349=ORIENTED_EDGE('',*,*,#8442,.T.);
#12350=ORIENTED_EDGE('',*,*,#8606,.F.);
#12351=ORIENTED_EDGE('',*,*,#8607,.F.);
#12352=ORIENTED_EDGE('',*,*,#8608,.F.);
#12353=ORIENTED_EDGE('',*,*,#8607,.T.);
#12354=ORIENTED_EDGE('',*,*,#8609,.T.);
#12355=ORIENTED_EDGE('',*,*,#8604,.T.);
#12356=ORIENTED_EDGE('',*,*,#8441,.T.);
#12357=ORIENTED_EDGE('',*,*,#8610,.F.);
#12358=ORIENTED_EDGE('',*,*,#8611,.F.);
#12359=ORIENTED_EDGE('',*,*,#8612,.F.);
#12360=ORIENTED_EDGE('',*,*,#8611,.T.);
#12361=ORIENTED_EDGE('',*,*,#8613,.T.);
#12362=ORIENTED_EDGE('',*,*,#8608,.T.);
#12363=ORIENTED_EDGE('',*,*,#8440,.T.);
#12364=ORIENTED_EDGE('',*,*,#8614,.F.);
#12365=ORIENTED_EDGE('',*,*,#8615,.F.);
#12366=ORIENTED_EDGE('',*,*,#8616,.F.);
#12367=ORIENTED_EDGE('',*,*,#8530,.F.);
#12368=ORIENTED_EDGE('',*,*,#8617,.T.);
#12369=ORIENTED_EDGE('',*,*,#8618,.T.);
#12370=ORIENTED_EDGE('',*,*,#8615,.T.);
#12371=ORIENTED_EDGE('',*,*,#8438,.T.);
#12372=ORIENTED_EDGE('',*,*,#8499,.T.);
#12373=ORIENTED_EDGE('',*,*,#8619,.T.);
#12374=ORIENTED_EDGE('',*,*,#8616,.T.);
#12375=ORIENTED_EDGE('',*,*,#8620,.T.);
#12376=ORIENTED_EDGE('',*,*,#8614,.T.);
#12377=ORIENTED_EDGE('',*,*,#8621,.T.);
#12378=ORIENTED_EDGE('',*,*,#8612,.T.);
#12379=ORIENTED_EDGE('',*,*,#8439,.T.);
#12380=ORIENTED_EDGE('',*,*,#8532,.F.);
#12381=ORIENTED_EDGE('',*,*,#8622,.T.);
#12382=ORIENTED_EDGE('',*,*,#8505,.T.);
#12383=ORIENTED_EDGE('',*,*,#8623,.T.);
#12384=ORIENTED_EDGE('',*,*,#8617,.F.);
#12385=ORIENTED_EDGE('',*,*,#8493,.T.);
#12386=ORIENTED_EDGE('',*,*,#8624,.T.);
#12387=ORIENTED_EDGE('',*,*,#8610,.T.);
#12388=ORIENTED_EDGE('',*,*,#8625,.T.);
#12389=ORIENTED_EDGE('',*,*,#8487,.T.);
#12390=ORIENTED_EDGE('',*,*,#8626,.T.);
#12391=ORIENTED_EDGE('',*,*,#8606,.T.);
#12392=ORIENTED_EDGE('',*,*,#8627,.T.);
#12393=ORIENTED_EDGE('',*,*,#8481,.T.);
#12394=ORIENTED_EDGE('',*,*,#8628,.T.);
#12395=ORIENTED_EDGE('',*,*,#8602,.T.);
#12396=ORIENTED_EDGE('',*,*,#8629,.T.);
#12397=ORIENTED_EDGE('',*,*,#8475,.T.);
#12398=ORIENTED_EDGE('',*,*,#8630,.T.);
#12399=ORIENTED_EDGE('',*,*,#8600,.T.);
#12400=ORIENTED_EDGE('',*,*,#8631,.T.);
#12401=ORIENTED_EDGE('',*,*,#8561,.F.);
#12402=ORIENTED_EDGE('',*,*,#8563,.F.);
#12403=ORIENTED_EDGE('',*,*,#8630,.F.);
#12404=ORIENTED_EDGE('',*,*,#8474,.F.);
#12405=ORIENTED_EDGE('',*,*,#8632,.T.);
#12406=ORIENTED_EDGE('',*,*,#8633,.T.);
#12407=ORIENTED_EDGE('',*,*,#8634,.T.);
#12408=ORIENTED_EDGE('',*,*,#8470,.F.);
#12409=ORIENTED_EDGE('',*,*,#8631,.F.);
#12410=ORIENTED_EDGE('',*,*,#8605,.F.);
#12411=ORIENTED_EDGE('',*,*,#8628,.F.);
#12412=ORIENTED_EDGE('',*,*,#8480,.F.);
#12413=ORIENTED_EDGE('',*,*,#8635,.T.);
#12414=ORIENTED_EDGE('',*,*,#8636,.T.);
#12415=ORIENTED_EDGE('',*,*,#8637,.T.);
#12416=ORIENTED_EDGE('',*,*,#8476,.F.);
#12417=ORIENTED_EDGE('',*,*,#8629,.F.);
#12418=ORIENTED_EDGE('',*,*,#8609,.F.);
#12419=ORIENTED_EDGE('',*,*,#8626,.F.);
#12420=ORIENTED_EDGE('',*,*,#8486,.F.);
#12421=ORIENTED_EDGE('',*,*,#8638,.T.);
#12422=ORIENTED_EDGE('',*,*,#8639,.T.);
#12423=ORIENTED_EDGE('',*,*,#8640,.T.);
#12424=ORIENTED_EDGE('',*,*,#8482,.F.);
#12425=ORIENTED_EDGE('',*,*,#8627,.F.);
#12426=ORIENTED_EDGE('',*,*,#8613,.F.);
#12427=ORIENTED_EDGE('',*,*,#8624,.F.);
#12428=ORIENTED_EDGE('',*,*,#8492,.F.);
#12429=ORIENTED_EDGE('',*,*,#8641,.T.);
#12430=ORIENTED_EDGE('',*,*,#8642,.T.);
#12431=ORIENTED_EDGE('',*,*,#8643,.T.);
#12432=ORIENTED_EDGE('',*,*,#8488,.F.);
#12433=ORIENTED_EDGE('',*,*,#8625,.F.);
#12434=ORIENTED_EDGE('',*,*,#8621,.F.);
#12435=ORIENTED_EDGE('',*,*,#8619,.F.);
#12436=ORIENTED_EDGE('',*,*,#8498,.F.);
#12437=ORIENTED_EDGE('',*,*,#8644,.T.);
#12438=ORIENTED_EDGE('',*,*,#8645,.T.);
#12439=ORIENTED_EDGE('',*,*,#8646,.T.);
#12440=ORIENTED_EDGE('',*,*,#8494,.F.);
#12441=ORIENTED_EDGE('',*,*,#8647,.T.);
#12442=ORIENTED_EDGE('',*,*,#8648,.T.);
#12443=ORIENTED_EDGE('',*,*,#8649,.T.);
#12444=ORIENTED_EDGE('',*,*,#8502,.T.);
#12445=ORIENTED_EDGE('',*,*,#8648,.F.);
#12446=ORIENTED_EDGE('',*,*,#8650,.F.);
#12447=ORIENTED_EDGE('',*,*,#8651,.T.);
#12448=ORIENTED_EDGE('',*,*,#8652,.T.);
#12449=ORIENTED_EDGE('',*,*,#8653,.F.);
#12450=ORIENTED_EDGE('',*,*,#8654,.F.);
#12451=ORIENTED_EDGE('',*,*,#8651,.F.);
#12452=ORIENTED_EDGE('',*,*,#8655,.F.);
#12453=ORIENTED_EDGE('',*,*,#8656,.F.);
#12454=ORIENTED_EDGE('',*,*,#8655,.T.);
#12455=ORIENTED_EDGE('',*,*,#8650,.T.);
#12456=ORIENTED_EDGE('',*,*,#8647,.F.);
#12457=ORIENTED_EDGE('',*,*,#8501,.F.);
#12458=ORIENTED_EDGE('',*,*,#8657,.F.);
#12459=ORIENTED_EDGE('',*,*,#8503,.F.);
#12460=ORIENTED_EDGE('',*,*,#8649,.F.);
#12461=ORIENTED_EDGE('',*,*,#8652,.F.);
#12462=ORIENTED_EDGE('',*,*,#8654,.T.);
#12463=ORIENTED_EDGE('',*,*,#8623,.F.);
#12464=ORIENTED_EDGE('',*,*,#8504,.F.);
#12465=ORIENTED_EDGE('',*,*,#8657,.T.);
#12466=ORIENTED_EDGE('',*,*,#8653,.T.);
#12467=ORIENTED_EDGE('',*,*,#8656,.T.);
#12468=ORIENTED_EDGE('',*,*,#8500,.F.);
#12469=ORIENTED_EDGE('',*,*,#8620,.F.);
#12470=ORIENTED_EDGE('',*,*,#8618,.F.);
#12471=ORIENTED_EDGE('',*,*,#8645,.F.);
#12472=ORIENTED_EDGE('',*,*,#8658,.F.);
#12473=ORIENTED_EDGE('',*,*,#8598,.F.);
#12474=ORIENTED_EDGE('',*,*,#8659,.F.);
#12475=ORIENTED_EDGE('',*,*,#8646,.F.);
#12476=ORIENTED_EDGE('',*,*,#8659,.T.);
#12477=ORIENTED_EDGE('',*,*,#8597,.T.);
#12478=ORIENTED_EDGE('',*,*,#8594,.F.);
#12479=ORIENTED_EDGE('',*,*,#8495,.F.);
#12480=ORIENTED_EDGE('',*,*,#8644,.F.);
#12481=ORIENTED_EDGE('',*,*,#8497,.F.);
#12482=ORIENTED_EDGE('',*,*,#8596,.F.);
#12483=ORIENTED_EDGE('',*,*,#8599,.F.);
#12484=ORIENTED_EDGE('',*,*,#8658,.T.);
#12485=ORIENTED_EDGE('',*,*,#8642,.F.);
#12486=ORIENTED_EDGE('',*,*,#8660,.F.);
#12487=ORIENTED_EDGE('',*,*,#8592,.F.);
#12488=ORIENTED_EDGE('',*,*,#8661,.F.);
#12489=ORIENTED_EDGE('',*,*,#8643,.F.);
#12490=ORIENTED_EDGE('',*,*,#8661,.T.);
#12491=ORIENTED_EDGE('',*,*,#8591,.T.);
#12492=ORIENTED_EDGE('',*,*,#8588,.F.);
#12493=ORIENTED_EDGE('',*,*,#8489,.F.);
#12494=ORIENTED_EDGE('',*,*,#8641,.F.);
#12495=ORIENTED_EDGE('',*,*,#8491,.F.);
#12496=ORIENTED_EDGE('',*,*,#8590,.F.);
#12497=ORIENTED_EDGE('',*,*,#8593,.F.);
#12498=ORIENTED_EDGE('',*,*,#8660,.T.);
#12499=ORIENTED_EDGE('',*,*,#8639,.F.);
#12500=ORIENTED_EDGE('',*,*,#8662,.F.);
#12501=ORIENTED_EDGE('',*,*,#8586,.F.);
#12502=ORIENTED_EDGE('',*,*,#8663,.F.);
#12503=ORIENTED_EDGE('',*,*,#8640,.F.);
#12504=ORIENTED_EDGE('',*,*,#8663,.T.);
#12505=ORIENTED_EDGE('',*,*,#8585,.T.);
#12506=ORIENTED_EDGE('',*,*,#8582,.F.);
#12507=ORIENTED_EDGE('',*,*,#8483,.F.);
#12508=ORIENTED_EDGE('',*,*,#8638,.F.);
#12509=ORIENTED_EDGE('',*,*,#8485,.F.);
#12510=ORIENTED_EDGE('',*,*,#8584,.F.);
#12511=ORIENTED_EDGE('',*,*,#8587,.F.);
#12512=ORIENTED_EDGE('',*,*,#8662,.T.);
#12513=ORIENTED_EDGE('',*,*,#8636,.F.);
#12514=ORIENTED_EDGE('',*,*,#8664,.F.);
#12515=ORIENTED_EDGE('',*,*,#8580,.F.);
#12516=ORIENTED_EDGE('',*,*,#8665,.F.);
#12517=ORIENTED_EDGE('',*,*,#8637,.F.);
#12518=ORIENTED_EDGE('',*,*,#8665,.T.);
#12519=ORIENTED_EDGE('',*,*,#8579,.T.);
#12520=ORIENTED_EDGE('',*,*,#8576,.F.);
#12521=ORIENTED_EDGE('',*,*,#8477,.F.);
#12522=ORIENTED_EDGE('',*,*,#8635,.F.);
#12523=ORIENTED_EDGE('',*,*,#8479,.F.);
#12524=ORIENTED_EDGE('',*,*,#8578,.F.);
#12525=ORIENTED_EDGE('',*,*,#8581,.F.);
#12526=ORIENTED_EDGE('',*,*,#8664,.T.);
#12527=ORIENTED_EDGE('',*,*,#8633,.F.);
#12528=ORIENTED_EDGE('',*,*,#8666,.F.);
#12529=ORIENTED_EDGE('',*,*,#8574,.F.);
#12530=ORIENTED_EDGE('',*,*,#8667,.F.);
#12531=ORIENTED_EDGE('',*,*,#8634,.F.);
#12532=ORIENTED_EDGE('',*,*,#8667,.T.);
#12533=ORIENTED_EDGE('',*,*,#8573,.T.);
#12534=ORIENTED_EDGE('',*,*,#8570,.F.);
#12535=ORIENTED_EDGE('',*,*,#8471,.F.);
#12536=ORIENTED_EDGE('',*,*,#8632,.F.);
#12537=ORIENTED_EDGE('',*,*,#8473,.F.);
#12538=ORIENTED_EDGE('',*,*,#8572,.F.);
#12539=ORIENTED_EDGE('',*,*,#8575,.F.);
#12540=ORIENTED_EDGE('',*,*,#8666,.T.);
#12541=ORIENTED_EDGE('',*,*,#8558,.F.);
#12542=ORIENTED_EDGE('',*,*,#8668,.F.);
#12543=ORIENTED_EDGE('',*,*,#8568,.F.);
#12544=ORIENTED_EDGE('',*,*,#8669,.F.);
#12545=ORIENTED_EDGE('',*,*,#8559,.F.);
#12546=ORIENTED_EDGE('',*,*,#8669,.T.);
#12547=ORIENTED_EDGE('',*,*,#8567,.T.);
#12548=ORIENTED_EDGE('',*,*,#8564,.F.);
#12549=ORIENTED_EDGE('',*,*,#8465,.F.);
#12550=ORIENTED_EDGE('',*,*,#8557,.F.);
#12551=ORIENTED_EDGE('',*,*,#8467,.F.);
#12552=ORIENTED_EDGE('',*,*,#8566,.F.);
#12553=ORIENTED_EDGE('',*,*,#8569,.F.);
#12554=ORIENTED_EDGE('',*,*,#8668,.T.);
#12555=ORIENTED_EDGE('',*,*,#8554,.F.);
#12556=ORIENTED_EDGE('',*,*,#8670,.F.);
#12557=ORIENTED_EDGE('',*,*,#8525,.F.);
#12558=ORIENTED_EDGE('',*,*,#8671,.F.);
#12559=ORIENTED_EDGE('',*,*,#8555,.F.);
#12560=ORIENTED_EDGE('',*,*,#8671,.T.);
#12561=ORIENTED_EDGE('',*,*,#8524,.T.);
#12562=ORIENTED_EDGE('',*,*,#8521,.F.);
#12563=ORIENTED_EDGE('',*,*,#8459,.F.);
#12564=ORIENTED_EDGE('',*,*,#8553,.F.);
#12565=ORIENTED_EDGE('',*,*,#8461,.F.);
#12566=ORIENTED_EDGE('',*,*,#8523,.F.);
#12567=ORIENTED_EDGE('',*,*,#8526,.F.);
#12568=ORIENTED_EDGE('',*,*,#8670,.T.);
#12569=ORIENTED_EDGE('',*,*,#8551,.F.);
#12570=ORIENTED_EDGE('',*,*,#8672,.F.);
#12571=ORIENTED_EDGE('',*,*,#8519,.F.);
#12572=ORIENTED_EDGE('',*,*,#8673,.F.);
#12573=ORIENTED_EDGE('',*,*,#8552,.F.);
#12574=ORIENTED_EDGE('',*,*,#8673,.T.);
#12575=ORIENTED_EDGE('',*,*,#8518,.T.);
#12576=ORIENTED_EDGE('',*,*,#8515,.F.);
#12577=ORIENTED_EDGE('',*,*,#8453,.F.);
#12578=ORIENTED_EDGE('',*,*,#8550,.F.);
#12579=ORIENTED_EDGE('',*,*,#8455,.F.);
#12580=ORIENTED_EDGE('',*,*,#8517,.F.);
#12581=ORIENTED_EDGE('',*,*,#8520,.F.);
#12582=ORIENTED_EDGE('',*,*,#8672,.T.);
#12583=ORIENTED_EDGE('',*,*,#8674,.F.);
#12584=ORIENTED_EDGE('',*,*,#8675,.T.);
#12585=ORIENTED_EDGE('',*,*,#8512,.T.);
#12586=ORIENTED_EDGE('',*,*,#8509,.F.);
#12587=ORIENTED_EDGE('',*,*,#8507,.F.);
#12588=ORIENTED_EDGE('',*,*,#8676,.F.);
#12589=ORIENTED_EDGE('',*,*,#8449,.F.);
#12590=ORIENTED_EDGE('',*,*,#8511,.F.);
#12591=ORIENTED_EDGE('',*,*,#8514,.F.);
#12592=ORIENTED_EDGE('',*,*,#8677,.T.);
#12593=ORIENTED_EDGE('',*,*,#8678,.F.);
#12594=ORIENTED_EDGE('',*,*,#8677,.F.);
#12595=ORIENTED_EDGE('',*,*,#8513,.F.);
#12596=ORIENTED_EDGE('',*,*,#8675,.F.);
#12597=ORIENTED_EDGE('',*,*,#8548,.F.);
#12598=ORIENTED_EDGE('',*,*,#8450,.F.);
#12599=ORIENTED_EDGE('',*,*,#8676,.T.);
#12600=ORIENTED_EDGE('',*,*,#8678,.T.);
#12601=ORIENTED_EDGE('',*,*,#8674,.T.);
#12602=ORIENTED_EDGE('',*,*,#8506,.F.);
#12603=ORIENTED_EDGE('',*,*,#8622,.F.);
#12604=ORIENTED_EDGE('',*,*,#8531,.F.);
#12605=PLANE('',#13975);
#12606=PLANE('',#13979);
#12607=PLANE('',#13983);
#12608=PLANE('',#13987);
#12609=PLANE('',#13993);
#12610=PLANE('',#13997);
#12611=PLANE('',#13998);
#12612=PLANE('',#14003);
#12613=PLANE('',#14006);
#12614=PLANE('',#14009);
#12615=PLANE('',#14012);
#12616=PLANE('',#14017);
#12617=PLANE('',#14020);
#12618=PLANE('',#14021);
#12619=PLANE('',#14024);
#12620=PLANE('',#14028);
#12621=PLANE('',#14032);
#12622=PLANE('',#14036);
#12623=PLANE('',#14041);
#12624=PLANE('',#14043);
#12625=PLANE('',#14046);
#12626=PLANE('',#14049);
#12627=PLANE('',#14054);
#12628=PLANE('',#14056);
#12629=PLANE('',#14057);
#12630=PLANE('',#14059);
#12631=PLANE('',#14065);
#12632=PLANE('',#14071);
#12633=PLANE('',#14081);
#12634=PLANE('',#14086);
#12635=PLANE('',#14090);
#12636=PLANE('',#14093);
#12637=PLANE('',#14096);
#12638=PLANE('',#14098);
#12639=PLANE('',#14100);
#12640=PLANE('',#14101);
#12641=PLANE('',#14103);
#12642=PLANE('',#14105);
#12643=PLANE('',#14106);
#12644=PLANE('',#14108);
#12645=PLANE('',#14111);
#12646=PLANE('',#14113);
#12647=PLANE('',#14120);
#12648=PLANE('',#14123);
#12649=PLANE('',#14124);
#12650=PLANE('',#14128);
#12651=PLANE('',#14132);
#12652=PLANE('',#14136);
#12653=PLANE('',#14142);
#12654=PLANE('',#14145);
#12655=PLANE('',#14146);
#12656=PLANE('',#14153);
#12657=PLANE('',#14156);
#12658=PLANE('',#14159);
#12659=PLANE('',#14162);
#12660=PLANE('',#14163);
#12661=PLANE('',#14166);
#12662=PLANE('',#14169);
#12663=PLANE('',#14172);
#12664=PLANE('',#14175);
#12665=PLANE('',#14179);
#12666=PLANE('',#14183);
#12667=PLANE('',#14188);
#12668=PLANE('',#14190);
#12669=PLANE('',#14193);
#12670=PLANE('',#14196);
#12671=PLANE('',#14200);
#12672=PLANE('',#14202);
#12673=PLANE('',#14208);
#12674=PLANE('',#14239);
#12675=PLANE('',#14248);
#12676=PLANE('',#14252);
#12677=PLANE('',#14256);
#12678=PLANE('',#14260);
#12679=PLANE('',#14268);
#12680=PLANE('',#14299);
#12681=PLANE('',#14312);
#12682=PLANE('',#14315);
#12683=PLANE('',#14318);
#12684=PLANE('',#14321);
#12685=PLANE('',#14328);
#12686=PLANE('',#14341);
#12687=PLANE('',#14344);
#12688=PLANE('',#14348);
#12689=PLANE('',#14352);
#12690=PLANE('',#14356);
#12691=PLANE('',#14361);
#12692=PLANE('',#14363);
#12693=PLANE('',#14366);
#12694=PLANE('',#14369);
#12695=PLANE('',#14372);
#12696=PLANE('',#14374);
#12697=PLANE('',#14375);
#12698=PLANE('',#14377);
#12699=PLANE('',#14383);
#12700=PLANE('',#14389);
#12701=PLANE('',#14391);
#12702=PLANE('',#14397);
#12703=PLANE('',#14401);
#12704=PLANE('',#14410);
#12705=PLANE('',#14414);
#12706=PLANE('',#14415);
#12707=PLANE('',#14417);
#12708=PLANE('',#14419);
#12709=PLANE('',#14420);
#12710=PLANE('',#14422);
#12711=PLANE('',#14424);
#12712=PLANE('',#14425);
#12713=PLANE('',#14427);
#12714=PLANE('',#14430);
#12715=PLANE('',#14436);
#12716=PLANE('',#14444);
#12717=PLANE('',#14453);
#12718=PLANE('',#14463);
#12719=PLANE('',#14471);
#12720=PLANE('',#14477);
#12721=PLANE('',#14481);
#12722=PLANE('',#14485);
#12723=PLANE('',#14486);
#12724=PLANE('',#14489);
#12725=PLANE('',#14492);
#12726=PLANE('',#14493);
#12727=PLANE('',#14497);
#12728=PLANE('',#14501);
#12729=PLANE('',#14504);
#12730=PLANE('',#14509);
#12731=PLANE('',#14511);
#12732=PLANE('',#14513);
#12733=PLANE('',#14516);
#12734=PLANE('',#14519);
#12735=PLANE('',#14520);
#12736=PLANE('',#14521);
#12737=PLANE('',#14524);
#12738=PLANE('',#14527);
#12739=PLANE('',#14530);
#12740=PLANE('',#14533);
#12741=PLANE('',#14534);
#12742=PLANE('',#14535);
#12743=PLANE('',#14536);
#12744=PLANE('',#14540);
#12745=PLANE('',#14543);
#12746=PLANE('',#14544);
#12747=PLANE('',#14545);
#12748=PLANE('',#14548);
#12749=PLANE('',#14551);
#12750=PLANE('',#14552);
#12751=PLANE('',#14553);
#12752=PLANE('',#14554);
#12753=PLANE('',#14555);
#12754=PLANE('',#14556);
#12755=PLANE('',#14557);
#12756=PLANE('',#14558);
#12757=PLANE('',#14560);
#12758=PLANE('',#14561);
#12759=PLANE('',#14562);
#12760=PLANE('',#14563);
#12761=PLANE('',#14564);
#12762=PLANE('',#14565);
#12763=PLANE('',#14567);
#12764=PLANE('',#14568);
#12765=PLANE('',#14569);
#12766=PLANE('',#14570);
#12767=PLANE('',#14571);
#12768=PLANE('',#14572);
#12769=PLANE('',#14574);
#12770=PLANE('',#14575);
#12771=PLANE('',#14576);
#12772=PLANE('',#14577);
#12773=PLANE('',#14578);
#12774=PLANE('',#14579);
#12775=PLANE('',#14590);
#12776=PLANE('',#14591);
#12777=PLANE('',#14592);
#12778=PLANE('',#14593);
#12779=PLANE('',#14594);
#12780=PLANE('',#14595);
#12781=PLANE('',#14596);
#12782=PLANE('',#14597);
#12783=PLANE('',#14598);
#12784=PLANE('',#14599);
#12785=PLANE('',#14600);
#12786=PLANE('',#14601);
#12787=PLANE('',#14602);
#12788=PLANE('',#14604);
#12789=PLANE('',#14605);
#12790=PLANE('',#14606);
#12791=PLANE('',#14607);
#12792=PLANE('',#14608);
#12793=PLANE('',#14609);
#12794=PLANE('',#14618);
#12795=PLANE('',#14624);
#12796=PLANE('',#14628);
#12797=PLANE('',#14636);
#12798=PLANE('',#14638);
#12799=PLANE('',#14639);
#12800=PLANE('',#14640);
#12801=PLANE('',#14641);
#12802=PLANE('',#14642);
#12803=PLANE('',#14643);
#12804=PLANE('',#14644);
#12805=PLANE('',#14645);
#12806=PLANE('',#14646);
#12807=PLANE('',#14647);
#12808=PLANE('',#14648);
#12809=PLANE('',#14649);
#12810=PLANE('',#14650);
#12811=PLANE('',#14651);
#12812=PLANE('',#14652);
#12813=PLANE('',#14653);
#12814=PLANE('',#14654);
#12815=PLANE('',#14655);
#12816=PLANE('',#14656);
#12817=PLANE('',#14657);
#12818=PLANE('',#14658);
#12819=PLANE('',#14659);
#12820=PLANE('',#14660);
#12821=PLANE('',#14661);
#12822=PLANE('',#14662);
#12823=PLANE('',#14663);
#12824=PLANE('',#14664);
#12825=PLANE('',#14665);
#12826=PLANE('',#14666);
#12827=PLANE('',#14667);
#12828=PLANE('',#14668);
#12829=PLANE('',#14669);
#12830=PLANE('',#14670);
#12831=PLANE('',#14671);
#12832=PLANE('',#14672);
#12833=PLANE('',#14673);
#12834=PLANE('',#14674);
#12835=PLANE('',#14675);
#12836=PLANE('',#14676);
#12837=PLANE('',#14677);
#12838=PLANE('',#14678);
#12839=PLANE('',#14679);
#12840=PLANE('',#14680);
#12841=PLANE('',#14681);
#12842=PLANE('',#14682);
#12843=PLANE('',#14683);
#12844=PLANE('',#14684);
#12845=PLANE('',#14685);
#12846=PLANE('',#14686);
#12847=PLANE('',#14687);
#12848=PLANE('',#14688);
#12849=PLANE('',#14689);
#12850=PLANE('',#14691);
#12851=PLANE('',#14695);
#12852=PLANE('',#14699);
#12853=PLANE('',#14703);
#12854=PLANE('',#14709);
#12855=PLANE('',#14712);
#12856=PLANE('',#14713);
#12857=PLANE('',#14721);
#12858=PLANE('',#14725);
#12859=PLANE('',#14729);
#12860=PLANE('',#14733);
#12861=PLANE('',#14734);
#12862=PLANE('',#14736);
#12863=PLANE('',#14738);
#12864=PLANE('',#14745);
#12865=PLANE('',#14748);
#12866=PLANE('',#14751);
#12867=PLANE('',#14754);
#12868=PLANE('',#14755);
#12869=PLANE('',#14758);
#12870=PLANE('',#14770);
#12871=PLANE('',#14774);
#12872=PLANE('',#14777);
#12873=PLANE('',#14781);
#12874=PLANE('',#14785);
#12875=PLANE('',#14786);
#12876=PLANE('',#14793);
#12877=PLANE('',#14794);
#12878=PLANE('',#14796);
#12879=PLANE('',#14798);
#12880=PLANE('',#14800);
#12881=PLANE('',#14803);
#12882=PLANE('',#14807);
#12883=PLANE('',#14811);
#12884=PLANE('',#14815);
#12885=PLANE('',#14819);
#12886=PLANE('',#14826);
#12887=PLANE('',#14829);
#12888=PLANE('',#14830);
#12889=PLANE('',#14831);
#12890=PLANE('',#14832);
#12891=PLANE('',#14833);
#12892=PLANE('',#14834);
#12893=PLANE('',#14835);
#12894=PLANE('',#14836);
#12895=PLANE('',#14837);
#12896=PLANE('',#14842);
#12897=PLANE('',#14848);
#12898=PLANE('',#14851);
#12899=PLANE('',#14852);
#12900=PLANE('',#14853);
#12901=PLANE('',#14856);
#12902=PLANE('',#14859);
#12903=PLANE('',#14861);
#12904=PLANE('',#14864);
#12905=PLANE('',#14865);
#12906=PLANE('',#14866);
#12907=PLANE('',#14868);
#12908=PLANE('',#14871);
#12909=PLANE('',#14872);
#12910=PLANE('',#14876);
#12911=PLANE('',#14881);
#12912=PLANE('',#14884);
#12913=PLANE('',#14887);
#12914=PLANE('',#14888);
#12915=PLANE('',#14895);
#12916=PLANE('',#14898);
#12917=PLANE('',#14899);
#12918=PLANE('',#14900);
#12919=PLANE('',#14901);
#12920=PLANE('',#14902);
#12921=PLANE('',#14903);
#12922=PLANE('',#14904);
#12923=PLANE('',#14905);
#12924=PLANE('',#14906);
#12925=PLANE('',#14907);
#12926=PLANE('',#14908);
#12927=PLANE('',#14909);
#12928=PLANE('',#14910);
#12929=PLANE('',#14911);
#12930=PLANE('',#14912);
#12931=PLANE('',#14913);
#12932=PLANE('',#14914);
#12933=PLANE('',#14915);
#12934=PLANE('',#14916);
#12935=PLANE('',#14917);
#12936=PLANE('',#14918);
#12937=PLANE('',#14919);
#12938=PLANE('',#14920);
#12939=PLANE('',#14921);
#12940=PLANE('',#14922);
#12941=PLANE('',#14923);
#12942=PLANE('',#14924);
#12943=PLANE('',#14925);
#12944=PLANE('',#14926);
#12945=PLANE('',#14927);
#12946=PLANE('',#14928);
#12947=PLANE('',#14929);
#12948=PLANE('',#14930);
#12949=PLANE('',#14931);
#12950=PLANE('',#14932);
#12951=PLANE('',#14933);
#12952=PLANE('',#14934);
#12953=PLANE('',#14935);
#12954=PLANE('',#14936);
#12955=PLANE('',#14937);
#12956=PLANE('',#14938);
#12957=PLANE('',#14939);
#12958=PLANE('',#14940);
#12959=PLANE('',#14941);
#12960=PLANE('',#14942);
#12961=PLANE('',#14943);
#12962=PLANE('',#14944);
#12963=PLANE('',#14945);
#12964=PLANE('',#14946);
#12965=PLANE('',#14947);
#12966=PLANE('',#14948);
#12967=PLANE('',#14949);
#12968=PLANE('',#14950);
#12969=PLANE('',#14951);
#12970=PLANE('',#14952);
#12971=PLANE('',#14953);
#12972=PLANE('',#14954);
#12973=PLANE('',#14955);
#12974=PLANE('',#14956);
#12975=PLANE('',#14957);
#12976=PLANE('',#14958);
#12977=PLANE('',#14959);
#12978=PLANE('',#14960);
#12979=PLANE('',#14961);
#12980=PLANE('',#14962);
#12981=PLANE('',#14963);
#12982=PLANE('',#14964);
#12983=PLANE('',#14965);
#12984=PLANE('',#14966);
#12985=PLANE('',#14967);
#12986=PLANE('',#14968);
#12987=PLANE('',#14969);
#12988=PLANE('',#14970);
#12989=PLANE('',#14971);
#12990=PLANE('',#14972);
#12991=PLANE('',#14973);
#12992=PLANE('',#14974);
#12993=PLANE('',#14975);
#12994=PLANE('',#14976);
#12995=PLANE('',#14977);
#12996=PLANE('',#14978);
#12997=PLANE('',#14979);
#12998=PLANE('',#14980);
#12999=PLANE('',#14981);
#13000=PLANE('',#14982);
#13001=PLANE('',#14983);
#13002=PLANE('',#14984);
#13003=PLANE('',#14985);
#13004=PLANE('',#14986);
#13005=ADVANCED_FACE('',(#1242),#12605,.T.);
#13006=ADVANCED_FACE('',(#1243),#1097,.F.);
#13007=ADVANCED_FACE('',(#1244),#12606,.T.);
#13008=ADVANCED_FACE('',(#1245),#1098,.F.);
#13009=ADVANCED_FACE('',(#1246),#12607,.T.);
#13010=ADVANCED_FACE('',(#1247),#1099,.F.);
#13011=ADVANCED_FACE('',(#1248),#12608,.T.);
#13012=ADVANCED_FACE('',(#1249),#1100,.F.);
#13013=ADVANCED_FACE('',(#1250),#647,.F.);
#13014=ADVANCED_FACE('',(#1251,#591),#12609,.T.);
#13015=ADVANCED_FACE('',(#1252),#648,.F.);
#13016=ADVANCED_FACE('',(#1253),#12610,.T.);
#13017=ADVANCED_FACE('',(#1254,#592),#12611,.T.);
#13018=ADVANCED_FACE('',(#1255),#12612,.T.);
#13019=ADVANCED_FACE('',(#1256),#1101,.T.);
#13020=ADVANCED_FACE('',(#1257),#12613,.T.);
#13021=ADVANCED_FACE('',(#1258),#1102,.T.);
#13022=ADVANCED_FACE('',(#1259),#12614,.T.);
#13023=ADVANCED_FACE('',(#1260),#1103,.T.);
#13024=ADVANCED_FACE('',(#1261),#12615,.T.);
#13025=ADVANCED_FACE('',(#1262),#1104,.T.);
#13026=ADVANCED_FACE('',(#1263),#649,.T.);
#13027=ADVANCED_FACE('',(#1264),#12616,.T.);
#13028=ADVANCED_FACE('',(#1265),#650,.T.);
#13029=ADVANCED_FACE('',(#1266),#12617,.T.);
#13030=ADVANCED_FACE('',(#1267),#12618,.T.);
#13031=ADVANCED_FACE('',(#1268),#1105,.T.);
#13032=ADVANCED_FACE('',(#1269),#12619,.T.);
#13033=ADVANCED_FACE('',(#1270),#1106,.T.);
#13034=ADVANCED_FACE('',(#1271),#12620,.T.);
#13035=ADVANCED_FACE('',(#1272),#1107,.T.);
#13036=ADVANCED_FACE('',(#1273),#12621,.T.);
#13037=ADVANCED_FACE('',(#1274),#1108,.T.);
#13038=ADVANCED_FACE('',(#1275),#651,.T.);
#13039=ADVANCED_FACE('',(#1276,#593),#12622,.F.);
#13040=ADVANCED_FACE('',(#1277),#12623,.T.);
#13041=ADVANCED_FACE('',(#1278),#1109,.F.);
#13042=ADVANCED_FACE('',(#1279),#12624,.T.);
#13043=ADVANCED_FACE('',(#1280),#1110,.F.);
#13044=ADVANCED_FACE('',(#1281),#12625,.T.);
#13045=ADVANCED_FACE('',(#1282),#1111,.F.);
#13046=ADVANCED_FACE('',(#1283),#12626,.T.);
#13047=ADVANCED_FACE('',(#1284),#1112,.F.);
#13048=ADVANCED_FACE('',(#1285),#652,.F.);
#13049=ADVANCED_FACE('',(#1286),#653,.F.);
#13050=ADVANCED_FACE('',(#1287),#12627,.T.);
#13051=ADVANCED_FACE('',(#1288),#654,.F.);
#13052=ADVANCED_FACE('',(#1289),#12628,.T.);
#13053=ADVANCED_FACE('',(#1290),#12629,.T.);
#13054=ADVANCED_FACE('',(#1291),#655,.T.);
#13055=ADVANCED_FACE('',(#1292,#594),#12630,.T.);
#13056=ADVANCED_FACE('',(#1293),#407,.T.);
#13057=ADVANCED_FACE('',(#1294),#408,.T.);
#13058=ADVANCED_FACE('',(#1295),#409,.T.);
#13059=ADVANCED_FACE('',(#1296),#1113,.T.);
#13060=ADVANCED_FACE('',(#1297),#410,.T.);
#13061=ADVANCED_FACE('',(#1298),#411,.T.);
#13062=ADVANCED_FACE('',(#1299),#412,.T.);
#13063=ADVANCED_FACE('',(#1300),#656,.T.);
#13064=ADVANCED_FACE('',(#1301),#12631,.T.);
#13065=ADVANCED_FACE('',(#1302),#657,.T.);
#13066=ADVANCED_FACE('',(#1303),#413,.T.);
#13067=ADVANCED_FACE('',(#1304),#414,.T.);
#13068=ADVANCED_FACE('',(#1305),#415,.T.);
#13069=ADVANCED_FACE('',(#1306),#1114,.T.);
#13070=ADVANCED_FACE('',(#1307),#416,.T.);
#13071=ADVANCED_FACE('',(#1308),#417,.T.);
#13072=ADVANCED_FACE('',(#1309),#418,.T.);
#13073=ADVANCED_FACE('',(#1310),#12632,.F.);
#13074=ADVANCED_FACE('',(#1311),#419,.T.);
#13075=ADVANCED_FACE('',(#1312),#420,.T.);
#13076=ADVANCED_FACE('',(#1313),#421,.T.);
#13077=ADVANCED_FACE('',(#1314),#1115,.T.);
#13078=ADVANCED_FACE('',(#1315),#422,.T.);
#13079=ADVANCED_FACE('',(#1316),#423,.T.);
#13080=ADVANCED_FACE('',(#1317),#424,.T.);
#13081=ADVANCED_FACE('',(#1318),#658,.T.);
#13082=ADVANCED_FACE('',(#1319),#659,.T.);
#13083=ADVANCED_FACE('',(#1320),#425,.T.);
#13084=ADVANCED_FACE('',(#1321),#426,.T.);
#13085=ADVANCED_FACE('',(#1322),#427,.T.);
#13086=ADVANCED_FACE('',(#1323),#1116,.T.);
#13087=ADVANCED_FACE('',(#1324),#428,.T.);
#13088=ADVANCED_FACE('',(#1325),#429,.T.);
#13089=ADVANCED_FACE('',(#1326),#430,.T.);
#13090=ADVANCED_FACE('',(#1327),#12633,.T.);
#13091=ADVANCED_FACE('',(#1328),#660,.T.);
#13092=ADVANCED_FACE('',(#1329),#661,.T.);
#13093=ADVANCED_FACE('',(#1330),#12634,.T.);
#13094=ADVANCED_FACE('',(#1331),#662,.T.);
#13095=ADVANCED_FACE('',(#1332),#663,.T.);
#13096=ADVANCED_FACE('',(#1333),#664,.T.);
#13097=ADVANCED_FACE('',(#1334),#12635,.T.);
#13098=ADVANCED_FACE('',(#1335),#665,.T.);
#13099=ADVANCED_FACE('',(#1336),#666,.T.);
#13100=ADVANCED_FACE('',(#1337),#12636,.T.);
#13101=ADVANCED_FACE('',(#1338),#667,.T.);
#13102=ADVANCED_FACE('',(#1339),#431,.T.);
#13103=ADVANCED_FACE('',(#1340),#432,.T.);
#13104=ADVANCED_FACE('',(#1341),#433,.T.);
#13105=ADVANCED_FACE('',(#1342),#12637,.T.);
#13106=ADVANCED_FACE('',(#1343),#434,.T.);
#13107=ADVANCED_FACE('',(#1344),#668,.T.);
#13108=ADVANCED_FACE('',(#1345),#12638,.T.);
#13109=ADVANCED_FACE('',(#1346),#669,.T.);
#13110=ADVANCED_FACE('',(#1347),#12639,.F.);
#13111=ADVANCED_FACE('',(#1348),#435,.T.);
#13112=ADVANCED_FACE('',(#1349),#436,.T.);
#13113=ADVANCED_FACE('',(#1350),#437,.T.);
#13114=ADVANCED_FACE('',(#1351),#12640,.T.);
#13115=ADVANCED_FACE('',(#1352),#438,.T.);
#13116=ADVANCED_FACE('',(#1353),#670,.T.);
#13117=ADVANCED_FACE('',(#1354),#12641,.T.);
#13118=ADVANCED_FACE('',(#1355),#671,.T.);
#13119=ADVANCED_FACE('',(#1356),#439,.T.);
#13120=ADVANCED_FACE('',(#1357),#440,.T.);
#13121=ADVANCED_FACE('',(#1358),#441,.T.);
#13122=ADVANCED_FACE('',(#1359),#12642,.T.);
#13123=ADVANCED_FACE('',(#1360),#442,.T.);
#13124=ADVANCED_FACE('',(#1361),#443,.T.);
#13125=ADVANCED_FACE('',(#1362),#444,.T.);
#13126=ADVANCED_FACE('',(#1363),#445,.T.);
#13127=ADVANCED_FACE('',(#1364),#12643,.T.);
#13128=ADVANCED_FACE('',(#1365),#446,.T.);
#13129=ADVANCED_FACE('',(#1366),#672,.T.);
#13130=ADVANCED_FACE('',(#1367),#12644,.T.);
#13131=ADVANCED_FACE('',(#1368),#673,.T.);
#13132=ADVANCED_FACE('',(#1369),#674,.T.);
#13133=ADVANCED_FACE('',(#1370),#12645,.T.);
#13134=ADVANCED_FACE('',(#1371),#675,.T.);
#13135=ADVANCED_FACE('',(#1372),#12646,.T.);
#13136=ADVANCED_FACE('',(#1373),#1117,.F.);
#13137=ADVANCED_FACE('',(#1374),#676,.F.);
#13138=ADVANCED_FACE('',(#1375,#595),#12647,.T.);
#13139=ADVANCED_FACE('',(#1376),#1118,.F.);
#13140=ADVANCED_FACE('',(#1377,#596),#12648,.T.);
#13141=ADVANCED_FACE('',(#1378),#12649,.T.);
#13142=ADVANCED_FACE('',(#1379),#1119,.F.);
#13143=ADVANCED_FACE('',(#1380),#12650,.T.);
#13144=ADVANCED_FACE('',(#1381),#1120,.F.);
#13145=ADVANCED_FACE('',(#1382),#12651,.T.);
#13146=ADVANCED_FACE('',(#1383),#1121,.F.);
#13147=ADVANCED_FACE('',(#1384),#12652,.T.);
#13148=ADVANCED_FACE('',(#1385),#1122,.F.);
#13149=ADVANCED_FACE('',(#1386),#677,.F.);
#13150=ADVANCED_FACE('',(#1387),#12653,.T.);
#13151=ADVANCED_FACE('',(#1388),#678,.F.);
#13152=ADVANCED_FACE('',(#1389),#12654,.T.);
#13153=ADVANCED_FACE('',(#1390,#597),#12655,.T.);
#13154=ADVANCED_FACE('',(#1391),#1123,.T.);
#13155=ADVANCED_FACE('',(#1392),#12656,.T.);
#13156=ADVANCED_FACE('',(#1393),#1124,.T.);
#13157=ADVANCED_FACE('',(#1394),#12657,.T.);
#13158=ADVANCED_FACE('',(#1395),#1125,.T.);
#13159=ADVANCED_FACE('',(#1396),#12658,.T.);
#13160=ADVANCED_FACE('',(#1397),#1126,.T.);
#13161=ADVANCED_FACE('',(#1398),#12659,.T.);
#13162=ADVANCED_FACE('',(#1399),#12660,.T.);
#13163=ADVANCED_FACE('',(#1400),#679,.T.);
#13164=ADVANCED_FACE('',(#1401),#12661,.T.);
#13165=ADVANCED_FACE('',(#1402),#680,.T.);
#13166=ADVANCED_FACE('',(#1403),#12662,.T.);
#13167=ADVANCED_FACE('',(#1404),#1127,.T.);
#13168=ADVANCED_FACE('',(#1405),#12663,.T.);
#13169=ADVANCED_FACE('',(#1406),#1128,.T.);
#13170=ADVANCED_FACE('',(#1407),#12664,.T.);
#13171=ADVANCED_FACE('',(#1408),#1129,.T.);
#13172=ADVANCED_FACE('',(#1409),#12665,.T.);
#13173=ADVANCED_FACE('',(#1410),#1130,.T.);
#13174=ADVANCED_FACE('',(#1411,#598),#12666,.F.);
#13175=ADVANCED_FACE('',(#1412),#12667,.T.);
#13176=ADVANCED_FACE('',(#1413),#1131,.F.);
#13177=ADVANCED_FACE('',(#1414),#12668,.T.);
#13178=ADVANCED_FACE('',(#1415),#1132,.F.);
#13179=ADVANCED_FACE('',(#1416),#12669,.T.);
#13180=ADVANCED_FACE('',(#1417),#1133,.F.);
#13181=ADVANCED_FACE('',(#1418),#12670,.T.);
#13182=ADVANCED_FACE('',(#1419),#1134,.F.);
#13183=ADVANCED_FACE('',(#1420),#681,.F.);
#13184=ADVANCED_FACE('',(#1421),#682,.F.);
#13185=ADVANCED_FACE('',(#1422),#12671,.T.);
#13186=ADVANCED_FACE('',(#1423),#683,.T.);
#13187=ADVANCED_FACE('',(#1424),#12672,.T.);
#13188=ADVANCED_FACE('',(#1425),#684,.T.);
#13189=ADVANCED_FACE('',(#1426),#1135,.F.);
#13190=ADVANCED_FACE('',(#1427,#599,#600,#601,#602,#603,#604),#12673,.T.);
#13191=ADVANCED_FACE('',(#1428),#685,.F.);
#13192=ADVANCED_FACE('',(#1429),#1136,.F.);
#13193=ADVANCED_FACE('',(#1430),#686,.F.);
#13194=ADVANCED_FACE('',(#1431),#1137,.F.);
#13195=ADVANCED_FACE('',(#1432),#687,.F.);
#13196=ADVANCED_FACE('',(#1433),#1138,.F.);
#13197=ADVANCED_FACE('',(#1434),#688,.F.);
#13198=ADVANCED_FACE('',(#1435),#1139,.F.);
#13199=ADVANCED_FACE('',(#1436),#689,.F.);
#13200=ADVANCED_FACE('',(#1437),#1140,.F.);
#13201=ADVANCED_FACE('',(#1438),#690,.F.);
#13202=ADVANCED_FACE('',(#1439),#1141,.F.);
#13203=ADVANCED_FACE('',(#1440,#605,#606,#607,#608,#609,#610,#611),#12674,
 .T.);
#13204=ADVANCED_FACE('',(#1441),#691,.F.);
#13205=ADVANCED_FACE('',(#1442),#12675,.T.);
#13206=ADVANCED_FACE('',(#1443),#1142,.F.);
#13207=ADVANCED_FACE('',(#1444),#12676,.T.);
#13208=ADVANCED_FACE('',(#1445),#1143,.F.);
#13209=ADVANCED_FACE('',(#1446),#12677,.T.);
#13210=ADVANCED_FACE('',(#1447),#1144,.F.);
#13211=ADVANCED_FACE('',(#1448),#12678,.T.);
#13212=ADVANCED_FACE('',(#1449),#1145,.F.);
#13213=ADVANCED_FACE('',(#1450),#692,.F.);
#13214=ADVANCED_FACE('',(#1451),#693,.F.);
#13215=ADVANCED_FACE('',(#1452,#612),#12679,.F.);
#13216=ADVANCED_FACE('',(#1453),#1146,.F.);
#13217=ADVANCED_FACE('',(#1454),#694,.F.);
#13218=ADVANCED_FACE('',(#1455),#1147,.F.);
#13219=ADVANCED_FACE('',(#1456),#695,.F.);
#13220=ADVANCED_FACE('',(#1457),#1148,.F.);
#13221=ADVANCED_FACE('',(#1458),#696,.F.);
#13222=ADVANCED_FACE('',(#1459),#1149,.F.);
#13223=ADVANCED_FACE('',(#1460),#697,.F.);
#13224=ADVANCED_FACE('',(#1461),#1150,.F.);
#13225=ADVANCED_FACE('',(#1462),#698,.F.);
#13226=ADVANCED_FACE('',(#1463),#1151,.F.);
#13227=ADVANCED_FACE('',(#1464),#699,.F.);
#13228=ADVANCED_FACE('',(#1465),#1152,.F.);
#13229=ADVANCED_FACE('',(#1466,#613,#614,#615,#616,#617,#618,#619),#12680,
 .T.);
#13230=ADVANCED_FACE('',(#1467),#1153,.F.);
#13231=ADVANCED_FACE('',(#1468),#1154,.F.);
#13232=ADVANCED_FACE('',(#1469),#1155,.F.);
#13233=ADVANCED_FACE('',(#1470),#1156,.F.);
#13234=ADVANCED_FACE('',(#1471),#1157,.F.);
#13235=ADVANCED_FACE('',(#1472),#1158,.F.);
#13236=ADVANCED_FACE('',(#1473),#12681,.T.);
#13237=ADVANCED_FACE('',(#1474),#1159,.T.);
#13238=ADVANCED_FACE('',(#1475),#12682,.T.);
#13239=ADVANCED_FACE('',(#1476),#1160,.T.);
#13240=ADVANCED_FACE('',(#1477),#12683,.T.);
#13241=ADVANCED_FACE('',(#1478),#1161,.T.);
#13242=ADVANCED_FACE('',(#1479),#12684,.T.);
#13243=ADVANCED_FACE('',(#1480),#1162,.T.);
#13244=ADVANCED_FACE('',(#1481),#700,.T.);
#13245=ADVANCED_FACE('',(#1482),#701,.T.);
#13246=ADVANCED_FACE('',(#1483,#620,#621,#622,#623,#624,#625),#12685,.T.);
#13247=ADVANCED_FACE('',(#1484),#1163,.F.);
#13248=ADVANCED_FACE('',(#1485),#1164,.F.);
#13249=ADVANCED_FACE('',(#1486),#1165,.F.);
#13250=ADVANCED_FACE('',(#1487),#1166,.F.);
#13251=ADVANCED_FACE('',(#1488),#1167,.F.);
#13252=ADVANCED_FACE('',(#1489),#1168,.F.);
#13253=ADVANCED_FACE('',(#1490),#12686,.T.);
#13254=ADVANCED_FACE('',(#1491),#1169,.T.);
#13255=ADVANCED_FACE('',(#1492),#12687,.T.);
#13256=ADVANCED_FACE('',(#1493),#1170,.T.);
#13257=ADVANCED_FACE('',(#1494),#12688,.T.);
#13258=ADVANCED_FACE('',(#1495),#1171,.T.);
#13259=ADVANCED_FACE('',(#1496),#12689,.T.);
#13260=ADVANCED_FACE('',(#1497),#1172,.T.);
#13261=ADVANCED_FACE('',(#1498),#702,.T.);
#13262=ADVANCED_FACE('',(#1499,#626),#12690,.T.);
#13263=ADVANCED_FACE('',(#1500),#12691,.T.);
#13264=ADVANCED_FACE('',(#1501),#1173,.F.);
#13265=ADVANCED_FACE('',(#1502),#12692,.T.);
#13266=ADVANCED_FACE('',(#1503),#1174,.F.);
#13267=ADVANCED_FACE('',(#1504),#12693,.T.);
#13268=ADVANCED_FACE('',(#1505),#1175,.F.);
#13269=ADVANCED_FACE('',(#1506),#12694,.T.);
#13270=ADVANCED_FACE('',(#1507),#1176,.F.);
#13271=ADVANCED_FACE('',(#1508),#703,.F.);
#13272=ADVANCED_FACE('',(#1509),#12695,.T.);
#13273=ADVANCED_FACE('',(#1510),#704,.F.);
#13274=ADVANCED_FACE('',(#1511),#12696,.T.);
#13275=ADVANCED_FACE('',(#1512),#12697,.T.);
#13276=ADVANCED_FACE('',(#1513),#705,.T.);
#13277=ADVANCED_FACE('',(#1514),#12698,.T.);
#13278=ADVANCED_FACE('',(#1515),#447,.T.);
#13279=ADVANCED_FACE('',(#1516),#448,.T.);
#13280=ADVANCED_FACE('',(#1517),#449,.T.);
#13281=ADVANCED_FACE('',(#1518),#1177,.T.);
#13282=ADVANCED_FACE('',(#1519),#450,.T.);
#13283=ADVANCED_FACE('',(#1520),#451,.T.);
#13284=ADVANCED_FACE('',(#1521),#452,.T.);
#13285=ADVANCED_FACE('',(#1522),#706,.T.);
#13286=ADVANCED_FACE('',(#1523),#12699,.T.);
#13287=ADVANCED_FACE('',(#1524),#707,.T.);
#13288=ADVANCED_FACE('',(#1525),#453,.T.);
#13289=ADVANCED_FACE('',(#1526),#454,.T.);
#13290=ADVANCED_FACE('',(#1527),#455,.T.);
#13291=ADVANCED_FACE('',(#1528),#1178,.T.);
#13292=ADVANCED_FACE('',(#1529),#456,.T.);
#13293=ADVANCED_FACE('',(#1530),#457,.T.);
#13294=ADVANCED_FACE('',(#1531),#458,.T.);
#13295=ADVANCED_FACE('',(#1532),#12700,.T.);
#13296=ADVANCED_FACE('',(#1533),#708,.T.);
#13297=ADVANCED_FACE('',(#1534),#12701,.T.);
#13298=ADVANCED_FACE('',(#1535),#459,.T.);
#13299=ADVANCED_FACE('',(#1536),#460,.T.);
#13300=ADVANCED_FACE('',(#1537),#461,.T.);
#13301=ADVANCED_FACE('',(#1538),#1179,.T.);
#13302=ADVANCED_FACE('',(#1539),#462,.T.);
#13303=ADVANCED_FACE('',(#1540),#463,.T.);
#13304=ADVANCED_FACE('',(#1541),#464,.T.);
#13305=ADVANCED_FACE('',(#1542),#709,.T.);
#13306=ADVANCED_FACE('',(#1543),#12702,.T.);
#13307=ADVANCED_FACE('',(#1544),#465,.T.);
#13308=ADVANCED_FACE('',(#1545),#466,.T.);
#13309=ADVANCED_FACE('',(#1546),#467,.T.);
#13310=ADVANCED_FACE('',(#1547),#1180,.T.);
#13311=ADVANCED_FACE('',(#1548),#468,.T.);
#13312=ADVANCED_FACE('',(#1549),#469,.T.);
#13313=ADVANCED_FACE('',(#1550),#470,.T.);
#13314=ADVANCED_FACE('',(#1551),#12703,.F.);
#13315=ADVANCED_FACE('',(#1552),#710,.T.);
#13316=ADVANCED_FACE('',(#1553),#711,.T.);
#13317=ADVANCED_FACE('',(#1554),#712,.T.);
#13318=ADVANCED_FACE('',(#1555),#713,.T.);
#13319=ADVANCED_FACE('',(#1556),#714,.T.);
#13320=ADVANCED_FACE('',(#1557),#715,.T.);
#13321=ADVANCED_FACE('',(#1558),#12704,.T.);
#13322=ADVANCED_FACE('',(#1559),#716,.T.);
#13323=ADVANCED_FACE('',(#1560),#717,.T.);
#13324=ADVANCED_FACE('',(#1561),#471,.T.);
#13325=ADVANCED_FACE('',(#1562),#472,.T.);
#13326=ADVANCED_FACE('',(#1563),#473,.T.);
#13327=ADVANCED_FACE('',(#1564),#12705,.T.);
#13328=ADVANCED_FACE('',(#1565),#474,.T.);
#13329=ADVANCED_FACE('',(#1566),#12706,.F.);
#13330=ADVANCED_FACE('',(#1567),#718,.T.);
#13331=ADVANCED_FACE('',(#1568),#12707,.T.);
#13332=ADVANCED_FACE('',(#1569),#719,.T.);
#13333=ADVANCED_FACE('',(#1570),#475,.T.);
#13334=ADVANCED_FACE('',(#1571),#476,.T.);
#13335=ADVANCED_FACE('',(#1572),#477,.T.);
#13336=ADVANCED_FACE('',(#1573),#12708,.T.);
#13337=ADVANCED_FACE('',(#1574),#478,.T.);
#13338=ADVANCED_FACE('',(#1575),#479,.T.);
#13339=ADVANCED_FACE('',(#1576),#480,.T.);
#13340=ADVANCED_FACE('',(#1577),#481,.T.);
#13341=ADVANCED_FACE('',(#1578),#12709,.T.);
#13342=ADVANCED_FACE('',(#1579),#482,.T.);
#13343=ADVANCED_FACE('',(#1580),#720,.T.);
#13344=ADVANCED_FACE('',(#1581),#12710,.T.);
#13345=ADVANCED_FACE('',(#1582),#721,.T.);
#13346=ADVANCED_FACE('',(#1583),#12711,.T.);
#13347=ADVANCED_FACE('',(#1584),#483,.T.);
#13348=ADVANCED_FACE('',(#1585),#484,.T.);
#13349=ADVANCED_FACE('',(#1586),#485,.T.);
#13350=ADVANCED_FACE('',(#1587),#12712,.T.);
#13351=ADVANCED_FACE('',(#1588),#486,.T.);
#13352=ADVANCED_FACE('',(#1589),#722,.T.);
#13353=ADVANCED_FACE('',(#1590),#12713,.T.);
#13354=ADVANCED_FACE('',(#1591),#723,.T.);
#13355=ADVANCED_FACE('',(#1592),#724,.T.);
#13356=ADVANCED_FACE('',(#1593),#12714,.T.);
#13357=ADVANCED_FACE('',(#1594),#725,.T.);
#13358=ADVANCED_FACE('',(#1595),#1181,.T.);
#13359=ADVANCED_FACE('',(#1596),#12715,.T.);
#13360=ADVANCED_FACE('',(#1597),#1182,.T.);
#13361=ADVANCED_FACE('',(#1598),#726,.T.);
#13362=ADVANCED_FACE('',(#1599,#627),#12716,.T.);
#13363=ADVANCED_FACE('',(#1600),#727,.T.);
#13364=ADVANCED_FACE('',(#1601),#1183,.F.);
#13365=ADVANCED_FACE('',(#1602,#628),#12717,.T.);
#13366=ADVANCED_FACE('',(#1603),#728,.F.);
#13367=ADVANCED_FACE('',(#1604),#1184,.T.);
#13368=ADVANCED_FACE('',(#1605),#12718,.T.);
#13369=ADVANCED_FACE('',(#1606),#1185,.T.);
#13370=ADVANCED_FACE('',(#1607),#729,.T.);
#13371=ADVANCED_FACE('',(#1608,#629),#12719,.T.);
#13372=ADVANCED_FACE('',(#1609),#730,.T.);
#13373=ADVANCED_FACE('',(#1610),#12720,.T.);
#13374=ADVANCED_FACE('',(#1611),#1186,.T.);
#13375=ADVANCED_FACE('',(#1612),#12721,.T.);
#13376=ADVANCED_FACE('',(#1613),#1187,.T.);
#13377=ADVANCED_FACE('',(#1614),#12722,.T.);
#13378=ADVANCED_FACE('',(#1615),#12723,.T.);
#13379=ADVANCED_FACE('',(#1616),#731,.T.);
#13380=ADVANCED_FACE('',(#1617),#12724,.T.);
#13381=ADVANCED_FACE('',(#1618),#732,.T.);
#13382=ADVANCED_FACE('',(#1619),#12725,.T.);
#13383=ADVANCED_FACE('',(#1620),#12726,.T.);
#13384=ADVANCED_FACE('',(#1621),#1188,.T.);
#13385=ADVANCED_FACE('',(#1622),#12727,.T.);
#13386=ADVANCED_FACE('',(#1623),#1189,.T.);
#13387=ADVANCED_FACE('',(#1624),#12728,.T.);
#13388=ADVANCED_FACE('',(#1625),#733,.T.);
#13389=ADVANCED_FACE('',(#1626),#12729,.T.);
#13390=ADVANCED_FACE('',(#1627),#734,.T.);
#13391=ADVANCED_FACE('',(#1628),#1190,.T.);
#13392=ADVANCED_FACE('',(#1629),#12730,.T.);
#13393=ADVANCED_FACE('',(#1630),#1191,.T.);
#13394=ADVANCED_FACE('',(#1631),#12731,.T.);
#13395=ADVANCED_FACE('',(#1632),#1192,.T.);
#13396=ADVANCED_FACE('',(#1633),#12732,.T.);
#13397=ADVANCED_FACE('',(#1634),#1193,.T.);
#13398=ADVANCED_FACE('',(#1635),#12733,.T.);
#13399=ADVANCED_FACE('',(#1636),#735,.T.);
#13400=ADVANCED_FACE('',(#1637),#12734,.T.);
#13401=ADVANCED_FACE('',(#1638),#12735,.F.);
#13402=ADVANCED_FACE('',(#1639),#12736,.T.);
#13403=ADVANCED_FACE('',(#1640),#1194,.T.);
#13404=ADVANCED_FACE('',(#1641),#12737,.T.);
#13405=ADVANCED_FACE('',(#1642),#1195,.T.);
#13406=ADVANCED_FACE('',(#1643),#12738,.T.);
#13407=ADVANCED_FACE('',(#1644),#1196,.T.);
#13408=ADVANCED_FACE('',(#1645),#12739,.T.);
#13409=ADVANCED_FACE('',(#1646),#1197,.T.);
#13410=ADVANCED_FACE('',(#1647),#12740,.T.);
#13411=ADVANCED_FACE('',(#1648),#12741,.T.);
#13412=ADVANCED_FACE('',(#1649,#630,#631,#632,#633),#12742,.F.);
#13413=ADVANCED_FACE('',(#1650),#12743,.T.);
#13414=ADVANCED_FACE('',(#1651),#1198,.T.);
#13415=ADVANCED_FACE('',(#1652),#12744,.T.);
#13416=ADVANCED_FACE('',(#1653),#1199,.T.);
#13417=ADVANCED_FACE('',(#1654),#12745,.T.);
#13418=ADVANCED_FACE('',(#1655),#12746,.F.);
#13419=ADVANCED_FACE('',(#1656),#12747,.T.);
#13420=ADVANCED_FACE('',(#1657),#1200,.T.);
#13421=ADVANCED_FACE('',(#1658),#12748,.T.);
#13422=ADVANCED_FACE('',(#1659),#1201,.T.);
#13423=ADVANCED_FACE('',(#1660),#12749,.T.);
#13424=ADVANCED_FACE('',(#1661),#12750,.F.);
#13425=ADVANCED_FACE('',(#1662),#12751,.T.);
#13426=ADVANCED_FACE('',(#1663),#12752,.T.);
#13427=ADVANCED_FACE('',(#1664),#12753,.T.);
#13428=ADVANCED_FACE('',(#1665),#12754,.T.);
#13429=ADVANCED_FACE('',(#1666),#12755,.F.);
#13430=ADVANCED_FACE('',(#1667,#634),#12756,.F.);
#13431=ADVANCED_FACE('',(#1668),#12757,.T.);
#13432=ADVANCED_FACE('',(#1669),#12758,.T.);
#13433=ADVANCED_FACE('',(#1670),#12759,.T.);
#13434=ADVANCED_FACE('',(#1671),#12760,.T.);
#13435=ADVANCED_FACE('',(#1672),#12761,.F.);
#13436=ADVANCED_FACE('',(#1673,#635),#12762,.F.);
#13437=ADVANCED_FACE('',(#1674),#12763,.T.);
#13438=ADVANCED_FACE('',(#1675),#12764,.T.);
#13439=ADVANCED_FACE('',(#1676),#12765,.T.);
#13440=ADVANCED_FACE('',(#1677),#12766,.T.);
#13441=ADVANCED_FACE('',(#1678),#12767,.F.);
#13442=ADVANCED_FACE('',(#1679,#636),#12768,.F.);
#13443=ADVANCED_FACE('',(#1680),#12769,.T.);
#13444=ADVANCED_FACE('',(#1681),#12770,.T.);
#13445=ADVANCED_FACE('',(#1682),#12771,.T.);
#13446=ADVANCED_FACE('',(#1683),#12772,.T.);
#13447=ADVANCED_FACE('',(#1684),#12773,.F.);
#13448=ADVANCED_FACE('',(#1685,#637),#12774,.F.);
#13449=ADVANCED_FACE('',(#1686),#736,.F.);
#13450=ADVANCED_FACE('',(#1687),#737,.F.);
#13451=ADVANCED_FACE('',(#1688),#738,.F.);
#13452=ADVANCED_FACE('',(#1689),#739,.F.);
#13453=ADVANCED_FACE('',(#1690),#740,.F.);
#13454=ADVANCED_FACE('',(#1691),#12775,.F.);
#13455=ADVANCED_FACE('',(#1692,#638),#12776,.F.);
#13456=ADVANCED_FACE('',(#1693),#12777,.F.);
#13457=ADVANCED_FACE('',(#1694),#12778,.F.);
#13458=ADVANCED_FACE('',(#1695,#639),#12779,.F.);
#13459=ADVANCED_FACE('',(#1696),#12780,.F.);
#13460=ADVANCED_FACE('',(#1697),#12781,.F.);
#13461=ADVANCED_FACE('',(#1698,#640),#12782,.F.);
#13462=ADVANCED_FACE('',(#1699),#12783,.F.);
#13463=ADVANCED_FACE('',(#1700),#12784,.F.);
#13464=ADVANCED_FACE('',(#1701,#641),#12785,.F.);
#13465=ADVANCED_FACE('',(#1702),#12786,.F.);
#13466=ADVANCED_FACE('',(#1703),#12787,.T.);
#13467=ADVANCED_FACE('',(#1704),#741,.T.);
#13468=ADVANCED_FACE('',(#1705),#12788,.T.);
#13469=ADVANCED_FACE('',(#1706),#12789,.T.);
#13470=ADVANCED_FACE('',(#1707),#12790,.T.);
#13471=ADVANCED_FACE('',(#1708),#12791,.T.);
#13472=ADVANCED_FACE('',(#1709),#12792,.F.);
#13473=ADVANCED_FACE('',(#1710),#12793,.F.);
#13474=ADVANCED_FACE('',(#1711),#1202,.T.);
#13475=ADVANCED_FACE('',(#1712),#1203,.T.);
#13476=ADVANCED_FACE('',(#1713),#12794,.T.);
#13477=ADVANCED_FACE('',(#1714),#1204,.T.);
#13478=ADVANCED_FACE('',(#1715),#742,.T.);
#13479=ADVANCED_FACE('',(#1716),#12795,.T.);
#13480=ADVANCED_FACE('',(#1717),#1205,.T.);
#13481=ADVANCED_FACE('',(#1718),#12796,.T.);
#13482=ADVANCED_FACE('',(#1719),#1206,.T.);
#13483=ADVANCED_FACE('',(#1720),#743,.T.);
#13484=ADVANCED_FACE('',(#1721),#1207,.T.);
#13485=ADVANCED_FACE('',(#1722),#12797,.T.);
#13486=ADVANCED_FACE('',(#1723),#12798,.T.);
#13487=ADVANCED_FACE('',(#1724),#12799,.T.);
#13488=ADVANCED_FACE('',(#1725),#12800,.T.);
#13489=ADVANCED_FACE('',(#1726),#12801,.T.);
#13490=ADVANCED_FACE('',(#1727),#12802,.T.);
#13491=ADVANCED_FACE('',(#1728),#12803,.T.);
#13492=ADVANCED_FACE('',(#1729),#12804,.T.);
#13493=ADVANCED_FACE('',(#1730),#12805,.T.);
#13494=ADVANCED_FACE('',(#1731),#12806,.T.);
#13495=ADVANCED_FACE('',(#1732),#12807,.T.);
#13496=ADVANCED_FACE('',(#1733),#12808,.T.);
#13497=ADVANCED_FACE('',(#1734),#12809,.T.);
#13498=ADVANCED_FACE('',(#1735),#12810,.T.);
#13499=ADVANCED_FACE('',(#1736),#12811,.T.);
#13500=ADVANCED_FACE('',(#1737),#12812,.T.);
#13501=ADVANCED_FACE('',(#1738),#12813,.T.);
#13502=ADVANCED_FACE('',(#1739),#12814,.T.);
#13503=ADVANCED_FACE('',(#1740),#12815,.T.);
#13504=ADVANCED_FACE('',(#1741),#12816,.T.);
#13505=ADVANCED_FACE('',(#1742),#12817,.T.);
#13506=ADVANCED_FACE('',(#1743),#12818,.T.);
#13507=ADVANCED_FACE('',(#1744),#12819,.T.);
#13508=ADVANCED_FACE('',(#1745),#12820,.T.);
#13509=ADVANCED_FACE('',(#1746),#12821,.T.);
#13510=ADVANCED_FACE('',(#1747),#12822,.T.);
#13511=ADVANCED_FACE('',(#1748),#12823,.T.);
#13512=ADVANCED_FACE('',(#1749),#12824,.T.);
#13513=ADVANCED_FACE('',(#1750),#12825,.T.);
#13514=ADVANCED_FACE('',(#1751),#12826,.T.);
#13515=ADVANCED_FACE('',(#1752),#12827,.T.);
#13516=ADVANCED_FACE('',(#1753),#12828,.T.);
#13517=ADVANCED_FACE('',(#1754),#12829,.T.);
#13518=ADVANCED_FACE('',(#1755),#12830,.T.);
#13519=ADVANCED_FACE('',(#1756),#12831,.T.);
#13520=ADVANCED_FACE('',(#1757),#12832,.T.);
#13521=ADVANCED_FACE('',(#1758),#12833,.T.);
#13522=ADVANCED_FACE('',(#1759),#12834,.T.);
#13523=ADVANCED_FACE('',(#1760),#12835,.T.);
#13524=ADVANCED_FACE('',(#1761),#12836,.T.);
#13525=ADVANCED_FACE('',(#1762),#12837,.T.);
#13526=ADVANCED_FACE('',(#1763),#12838,.T.);
#13527=ADVANCED_FACE('',(#1764),#12839,.T.);
#13528=ADVANCED_FACE('',(#1765),#12840,.T.);
#13529=ADVANCED_FACE('',(#1766),#12841,.T.);
#13530=ADVANCED_FACE('',(#1767),#12842,.T.);
#13531=ADVANCED_FACE('',(#1768),#12843,.T.);
#13532=ADVANCED_FACE('',(#1769),#12844,.T.);
#13533=ADVANCED_FACE('',(#1770),#12845,.T.);
#13534=ADVANCED_FACE('',(#1771),#12846,.T.);
#13535=ADVANCED_FACE('',(#1772),#12847,.T.);
#13536=ADVANCED_FACE('',(#1773),#12848,.T.);
#13537=ADVANCED_FACE('',(#1774),#12849,.F.);
#13538=ADVANCED_FACE('',(#1775),#12850,.T.);
#13539=ADVANCED_FACE('',(#1776),#1208,.F.);
#13540=ADVANCED_FACE('',(#1777),#12851,.T.);
#13541=ADVANCED_FACE('',(#1778),#1209,.F.);
#13542=ADVANCED_FACE('',(#1779),#12852,.T.);
#13543=ADVANCED_FACE('',(#1780),#1210,.F.);
#13544=ADVANCED_FACE('',(#1781),#12853,.T.);
#13545=ADVANCED_FACE('',(#1782),#1211,.F.);
#13546=ADVANCED_FACE('',(#1783),#744,.F.);
#13547=ADVANCED_FACE('',(#1784),#12854,.T.);
#13548=ADVANCED_FACE('',(#1785),#745,.F.);
#13549=ADVANCED_FACE('',(#1786),#12855,.T.);
#13550=ADVANCED_FACE('',(#1787,#642),#12856,.T.);
#13551=ADVANCED_FACE('',(#1788),#1212,.F.);
#13552=ADVANCED_FACE('',(#1789),#12857,.T.);
#13553=ADVANCED_FACE('',(#1790),#1213,.F.);
#13554=ADVANCED_FACE('',(#1791),#12858,.T.);
#13555=ADVANCED_FACE('',(#1792),#1214,.F.);
#13556=ADVANCED_FACE('',(#1793),#12859,.T.);
#13557=ADVANCED_FACE('',(#1794),#1215,.F.);
#13558=ADVANCED_FACE('',(#1795),#12860,.T.);
#13559=ADVANCED_FACE('',(#1796),#12861,.T.);
#13560=ADVANCED_FACE('',(#1797),#746,.F.);
#13561=ADVANCED_FACE('',(#1798),#12862,.T.);
#13562=ADVANCED_FACE('',(#1799),#747,.F.);
#13563=ADVANCED_FACE('',(#1800,#643),#12863,.T.);
#13564=ADVANCED_FACE('',(#1801),#1216,.T.);
#13565=ADVANCED_FACE('',(#1802),#12864,.T.);
#13566=ADVANCED_FACE('',(#1803),#1217,.T.);
#13567=ADVANCED_FACE('',(#1804),#12865,.T.);
#13568=ADVANCED_FACE('',(#1805),#1218,.T.);
#13569=ADVANCED_FACE('',(#1806),#12866,.T.);
#13570=ADVANCED_FACE('',(#1807),#1219,.T.);
#13571=ADVANCED_FACE('',(#1808),#12867,.T.);
#13572=ADVANCED_FACE('',(#1809),#12868,.T.);
#13573=ADVANCED_FACE('',(#1810),#748,.T.);
#13574=ADVANCED_FACE('',(#1811),#12869,.T.);
#13575=ADVANCED_FACE('',(#1812),#749,.T.);
#13576=ADVANCED_FACE('',(#1813),#487,.T.);
#13577=ADVANCED_FACE('',(#1814),#488,.T.);
#13578=ADVANCED_FACE('',(#1815),#489,.T.);
#13579=ADVANCED_FACE('',(#1816),#1220,.T.);
#13580=ADVANCED_FACE('',(#1817),#490,.T.);
#13581=ADVANCED_FACE('',(#1818),#491,.T.);
#13582=ADVANCED_FACE('',(#1819),#492,.T.);
#13583=ADVANCED_FACE('',(#1820),#750,.T.);
#13584=ADVANCED_FACE('',(#1821),#751,.T.);
#13585=ADVANCED_FACE('',(#1822),#493,.T.);
#13586=ADVANCED_FACE('',(#1823),#494,.T.);
#13587=ADVANCED_FACE('',(#1824),#495,.T.);
#13588=ADVANCED_FACE('',(#1825),#1221,.T.);
#13589=ADVANCED_FACE('',(#1826),#496,.T.);
#13590=ADVANCED_FACE('',(#1827),#497,.T.);
#13591=ADVANCED_FACE('',(#1828),#498,.T.);
#13592=ADVANCED_FACE('',(#1829),#752,.T.);
#13593=ADVANCED_FACE('',(#1830),#12870,.T.);
#13594=ADVANCED_FACE('',(#1831),#753,.T.);
#13595=ADVANCED_FACE('',(#1832),#1222,.F.);
#13596=ADVANCED_FACE('',(#1833),#12871,.T.);
#13597=ADVANCED_FACE('',(#1834),#1223,.F.);
#13598=ADVANCED_FACE('',(#1835),#12872,.T.);
#13599=ADVANCED_FACE('',(#1836),#1224,.F.);
#13600=ADVANCED_FACE('',(#1837),#12873,.T.);
#13601=ADVANCED_FACE('',(#1838),#1225,.F.);
#13602=ADVANCED_FACE('',(#1839),#12874,.T.);
#13603=ADVANCED_FACE('',(#1840,#644),#12875,.F.);
#13604=ADVANCED_FACE('',(#1841),#499,.T.);
#13605=ADVANCED_FACE('',(#1842),#500,.T.);
#13606=ADVANCED_FACE('',(#1843),#501,.T.);
#13607=ADVANCED_FACE('',(#1844),#1226,.T.);
#13608=ADVANCED_FACE('',(#1845),#502,.T.);
#13609=ADVANCED_FACE('',(#1846),#503,.T.);
#13610=ADVANCED_FACE('',(#1847),#504,.T.);
#13611=ADVANCED_FACE('',(#1848),#754,.T.);
#13612=ADVANCED_FACE('',(#1849),#505,.T.);
#13613=ADVANCED_FACE('',(#1850),#506,.T.);
#13614=ADVANCED_FACE('',(#1851),#507,.T.);
#13615=ADVANCED_FACE('',(#1852),#1227,.T.);
#13616=ADVANCED_FACE('',(#1853),#508,.T.);
#13617=ADVANCED_FACE('',(#1854),#509,.T.);
#13618=ADVANCED_FACE('',(#1855),#510,.T.);
#13619=ADVANCED_FACE('',(#1856),#755,.T.);
#13620=ADVANCED_FACE('',(#1857),#12876,.T.);
#13621=ADVANCED_FACE('',(#1858),#12877,.T.);
#13622=ADVANCED_FACE('',(#1859),#756,.F.);
#13623=ADVANCED_FACE('',(#1860),#12878,.T.);
#13624=ADVANCED_FACE('',(#1861),#757,.F.);
#13625=ADVANCED_FACE('',(#1862),#12879,.T.);
#13626=ADVANCED_FACE('',(#1863),#758,.F.);
#13627=ADVANCED_FACE('',(#1864),#12880,.T.);
#13628=ADVANCED_FACE('',(#1865),#759,.F.);
#13629=ADVANCED_FACE('',(#1866),#12881,.T.);
#13630=ADVANCED_FACE('',(#1867),#1228,.F.);
#13631=ADVANCED_FACE('',(#1868),#12882,.T.);
#13632=ADVANCED_FACE('',(#1869),#1229,.F.);
#13633=ADVANCED_FACE('',(#1870),#12883,.T.);
#13634=ADVANCED_FACE('',(#1871),#1230,.F.);
#13635=ADVANCED_FACE('',(#1872),#12884,.T.);
#13636=ADVANCED_FACE('',(#1873),#1231,.F.);
#13637=ADVANCED_FACE('',(#1874),#12885,.T.);
#13638=ADVANCED_FACE('',(#1875),#760,.F.);
#13639=ADVANCED_FACE('',(#1876),#12886,.F.);
#13640=ADVANCED_FACE('',(#1877),#761,.F.);
#13641=ADVANCED_FACE('',(#1878),#12887,.F.);
#13642=ADVANCED_FACE('',(#1879),#12888,.T.);
#13643=ADVANCED_FACE('',(#1880),#12889,.T.);
#13644=ADVANCED_FACE('',(#1881),#12890,.T.);
#13645=ADVANCED_FACE('',(#1882),#12891,.T.);
#13646=ADVANCED_FACE('',(#1883),#12892,.T.);
#13647=ADVANCED_FACE('',(#1884),#12893,.T.);
#13648=ADVANCED_FACE('',(#1885),#12894,.T.);
#13649=ADVANCED_FACE('',(#1886),#12895,.T.);
#13650=ADVANCED_FACE('',(#1887),#511,.T.);
#13651=ADVANCED_FACE('',(#1888),#512,.T.);
#13652=ADVANCED_FACE('',(#1889),#513,.T.);
#13653=ADVANCED_FACE('',(#1890),#1232,.T.);
#13654=ADVANCED_FACE('',(#1891),#514,.T.);
#13655=ADVANCED_FACE('',(#1892),#515,.T.);
#13656=ADVANCED_FACE('',(#1893),#516,.T.);
#13657=ADVANCED_FACE('',(#1894),#762,.T.);
#13658=ADVANCED_FACE('',(#1895),#12896,.T.);
#13659=ADVANCED_FACE('',(#1896),#763,.T.);
#13660=ADVANCED_FACE('',(#1897),#517,.T.);
#13661=ADVANCED_FACE('',(#1898),#518,.T.);
#13662=ADVANCED_FACE('',(#1899),#519,.T.);
#13663=ADVANCED_FACE('',(#1900),#1233,.T.);
#13664=ADVANCED_FACE('',(#1901),#520,.T.);
#13665=ADVANCED_FACE('',(#1902),#521,.T.);
#13666=ADVANCED_FACE('',(#1903),#522,.T.);
#13667=ADVANCED_FACE('',(#1904),#12897,.F.);
#13668=ADVANCED_FACE('',(#1905),#12898,.T.);
#13669=ADVANCED_FACE('',(#1906),#12899,.T.);
#13670=ADVANCED_FACE('',(#1907),#12900,.T.);
#13671=ADVANCED_FACE('',(#1908),#1234,.T.);
#13672=ADVANCED_FACE('',(#1909),#12901,.T.);
#13673=ADVANCED_FACE('',(#1910),#1235,.T.);
#13674=ADVANCED_FACE('',(#1911),#12902,.T.);
#13675=ADVANCED_FACE('',(#1912),#1236,.T.);
#13676=ADVANCED_FACE('',(#1913),#12903,.T.);
#13677=ADVANCED_FACE('',(#1914),#1237,.T.);
#13678=ADVANCED_FACE('',(#1915),#12904,.T.);
#13679=ADVANCED_FACE('',(#1916),#12905,.T.);
#13680=ADVANCED_FACE('',(#1917),#12906,.T.);
#13681=ADVANCED_FACE('',(#1918),#764,.T.);
#13682=ADVANCED_FACE('',(#1919),#12907,.T.);
#13683=ADVANCED_FACE('',(#1920),#765,.T.);
#13684=ADVANCED_FACE('',(#1921),#12908,.T.);
#13685=ADVANCED_FACE('',(#1922),#12909,.T.);
#13686=ADVANCED_FACE('',(#1923),#523,.T.);
#13687=ADVANCED_FACE('',(#1924),#524,.T.);
#13688=ADVANCED_FACE('',(#1925),#525,.T.);
#13689=ADVANCED_FACE('',(#1926),#1238,.T.);
#13690=ADVANCED_FACE('',(#1927),#526,.T.);
#13691=ADVANCED_FACE('',(#1928),#527,.T.);
#13692=ADVANCED_FACE('',(#1929),#528,.T.);
#13693=ADVANCED_FACE('',(#1930),#766,.T.);
#13694=ADVANCED_FACE('',(#1931),#12910,.T.);
#13695=ADVANCED_FACE('',(#1932),#767,.T.);
#13696=ADVANCED_FACE('',(#1933),#529,.T.);
#13697=ADVANCED_FACE('',(#1934),#530,.T.);
#13698=ADVANCED_FACE('',(#1935),#531,.T.);
#13699=ADVANCED_FACE('',(#1936),#1239,.T.);
#13700=ADVANCED_FACE('',(#1937),#532,.T.);
#13701=ADVANCED_FACE('',(#1938),#533,.T.);
#13702=ADVANCED_FACE('',(#1939),#534,.T.);
#13703=ADVANCED_FACE('',(#1940),#768,.T.);
#13704=ADVANCED_FACE('',(#1941),#769,.T.);
#13705=ADVANCED_FACE('',(#1942),#12911,.T.);
#13706=ADVANCED_FACE('',(#1943),#770,.F.);
#13707=ADVANCED_FACE('',(#1944),#12912,.F.);
#13708=ADVANCED_FACE('',(#1945),#771,.F.);
#13709=ADVANCED_FACE('',(#1946),#12913,.F.);
#13710=ADVANCED_FACE('',(#1947),#12914,.T.);
#13711=ADVANCED_FACE('',(#1948),#1240,.F.);
#13712=ADVANCED_FACE('',(#1949),#772,.F.);
#13713=ADVANCED_FACE('',(#1950,#645),#12915,.F.);
#13714=ADVANCED_FACE('',(#1951),#1241,.F.);
#13715=ADVANCED_FACE('',(#1952,#646),#12916,.T.);
#13716=ADVANCED_FACE('',(#1953),#12917,.T.);
#13717=ADVANCED_FACE('',(#1954),#12918,.F.);
#13718=ADVANCED_FACE('',(#1955),#12919,.T.);
#13719=ADVANCED_FACE('',(#1956),#12920,.F.);
#13720=ADVANCED_FACE('',(#1957),#12921,.T.);
#13721=ADVANCED_FACE('',(#1958),#12922,.F.);
#13722=ADVANCED_FACE('',(#1959),#12923,.T.);
#13723=ADVANCED_FACE('',(#1960),#12924,.T.);
#13724=ADVANCED_FACE('',(#1961),#12925,.T.);
#13725=ADVANCED_FACE('',(#1962),#12926,.T.);
#13726=ADVANCED_FACE('',(#1963),#12927,.T.);
#13727=ADVANCED_FACE('',(#1964),#12928,.T.);
#13728=ADVANCED_FACE('',(#1965),#12929,.T.);
#13729=ADVANCED_FACE('',(#1966),#12930,.T.);
#13730=ADVANCED_FACE('',(#1967),#12931,.T.);
#13731=ADVANCED_FACE('',(#1968),#12932,.T.);
#13732=ADVANCED_FACE('',(#1969),#12933,.T.);
#13733=ADVANCED_FACE('',(#1970),#12934,.T.);
#13734=ADVANCED_FACE('',(#1971),#12935,.T.);
#13735=ADVANCED_FACE('',(#1972),#12936,.T.);
#13736=ADVANCED_FACE('',(#1973),#12937,.T.);
#13737=ADVANCED_FACE('',(#1974),#12938,.T.);
#13738=ADVANCED_FACE('',(#1975),#12939,.F.);
#13739=ADVANCED_FACE('',(#1976),#12940,.T.);
#13740=ADVANCED_FACE('',(#1977),#12941,.F.);
#13741=ADVANCED_FACE('',(#1978),#12942,.T.);
#13742=ADVANCED_FACE('',(#1979),#12943,.F.);
#13743=ADVANCED_FACE('',(#1980),#12944,.T.);
#13744=ADVANCED_FACE('',(#1981),#12945,.F.);
#13745=ADVANCED_FACE('',(#1982),#12946,.T.);
#13746=ADVANCED_FACE('',(#1983),#12947,.F.);
#13747=ADVANCED_FACE('',(#1984),#12948,.T.);
#13748=ADVANCED_FACE('',(#1985),#12949,.F.);
#13749=ADVANCED_FACE('',(#1986),#12950,.T.);
#13750=ADVANCED_FACE('',(#1987),#12951,.T.);
#13751=ADVANCED_FACE('',(#1988),#12952,.T.);
#13752=ADVANCED_FACE('',(#1989),#12953,.T.);
#13753=ADVANCED_FACE('',(#1990),#12954,.T.);
#13754=ADVANCED_FACE('',(#1991),#12955,.T.);
#13755=ADVANCED_FACE('',(#1992),#12956,.T.);
#13756=ADVANCED_FACE('',(#1993),#12957,.T.);
#13757=ADVANCED_FACE('',(#1994),#12958,.T.);
#13758=ADVANCED_FACE('',(#1995),#12959,.T.);
#13759=ADVANCED_FACE('',(#1996),#12960,.T.);
#13760=ADVANCED_FACE('',(#1997),#12961,.T.);
#13761=ADVANCED_FACE('',(#1998),#12962,.T.);
#13762=ADVANCED_FACE('',(#1999),#12963,.T.);
#13763=ADVANCED_FACE('',(#2000),#12964,.T.);
#13764=ADVANCED_FACE('',(#2001),#12965,.T.);
#13765=ADVANCED_FACE('',(#2002),#12966,.T.);
#13766=ADVANCED_FACE('',(#2003),#12967,.T.);
#13767=ADVANCED_FACE('',(#2004),#12968,.T.);
#13768=ADVANCED_FACE('',(#2005),#12969,.T.);
#13769=ADVANCED_FACE('',(#2006),#12970,.T.);
#13770=ADVANCED_FACE('',(#2007),#12971,.T.);
#13771=ADVANCED_FACE('',(#2008),#12972,.F.);
#13772=ADVANCED_FACE('',(#2009),#12973,.T.);
#13773=ADVANCED_FACE('',(#2010),#12974,.F.);
#13774=ADVANCED_FACE('',(#2011),#12975,.F.);
#13775=ADVANCED_FACE('',(#2012),#12976,.T.);
#13776=ADVANCED_FACE('',(#2013),#12977,.T.);
#13777=ADVANCED_FACE('',(#2014),#12978,.F.);
#13778=ADVANCED_FACE('',(#2015),#12979,.F.);
#13779=ADVANCED_FACE('',(#2016),#12980,.T.);
#13780=ADVANCED_FACE('',(#2017),#12981,.F.);
#13781=ADVANCED_FACE('',(#2018),#12982,.F.);
#13782=ADVANCED_FACE('',(#2019),#12983,.T.);
#13783=ADVANCED_FACE('',(#2020),#12984,.F.);
#13784=ADVANCED_FACE('',(#2021),#12985,.F.);
#13785=ADVANCED_FACE('',(#2022),#12986,.T.);
#13786=ADVANCED_FACE('',(#2023),#12987,.F.);
#13787=ADVANCED_FACE('',(#2024),#12988,.F.);
#13788=ADVANCED_FACE('',(#2025),#12989,.T.);
#13789=ADVANCED_FACE('',(#2026),#12990,.F.);
#13790=ADVANCED_FACE('',(#2027),#12991,.F.);
#13791=ADVANCED_FACE('',(#2028),#12992,.T.);
#13792=ADVANCED_FACE('',(#2029),#12993,.F.);
#13793=ADVANCED_FACE('',(#2030),#12994,.F.);
#13794=ADVANCED_FACE('',(#2031),#12995,.T.);
#13795=ADVANCED_FACE('',(#2032),#12996,.F.);
#13796=ADVANCED_FACE('',(#2033),#12997,.F.);
#13797=ADVANCED_FACE('',(#2034),#12998,.T.);
#13798=ADVANCED_FACE('',(#2035),#12999,.F.);
#13799=ADVANCED_FACE('',(#2036),#13000,.F.);
#13800=ADVANCED_FACE('',(#2037),#13001,.F.);
#13801=ADVANCED_FACE('',(#2038),#13002,.F.);
#13802=ADVANCED_FACE('',(#2039),#13003,.T.);
#13803=ADVANCED_FACE('',(#2040),#13004,.T.);
#13804=CLOSED_SHELL('',(#13005,#13006,#13007,#13008,#13009,#13010,#13011,
#13012,#13013,#13014,#13015,#13016,#13017,#13018,#13019,#13020,#13021,#13022,
#13023,#13024,#13025,#13026,#13027,#13028,#13029,#13030,#13031,#13032,#13033,
#13034,#13035,#13036,#13037,#13038,#13039,#13040,#13041,#13042,#13043,#13044,
#13045,#13046,#13047,#13048,#13049,#13050,#13051,#13052,#13053,#13054,#13055));
#13805=CLOSED_SHELL('',(#13056,#13057,#13058,#13059,#13060,#13061,#13062,
#13063,#13064,#13065,#13066,#13067,#13068,#13069,#13070,#13071,#13072,#13073,
#13074,#13075,#13076,#13077,#13078,#13079,#13080,#13081,#13082,#13083,#13084,
#13085,#13086,#13087,#13088,#13089,#13090,#13091,#13092,#13093,#13094,#13095,
#13096,#13097,#13098,#13099,#13100,#13101));
#13806=CLOSED_SHELL('',(#13102,#13103,#13104,#13105,#13106,#13107,#13108,
#13109,#13110,#13111,#13112,#13113,#13114,#13115,#13116,#13117,#13118,#13119,
#13120,#13121,#13122,#13123,#13124,#13125,#13126,#13127,#13128,#13129,#13130,
#13131,#13132,#13133,#13134,#13135));
#13807=CLOSED_SHELL('',(#13136,#13137,#13138,#13139,#13140,#13141,#13142,
#13143,#13144,#13145,#13146,#13147,#13148,#13149,#13150,#13151,#13152,#13153,
#13154,#13155,#13156,#13157,#13158,#13159,#13160,#13161,#13162,#13163,#13164,
#13165,#13166,#13167,#13168,#13169,#13170,#13171,#13172,#13173,#13174,#13175,
#13176,#13177,#13178,#13179,#13180,#13181,#13182,#13183,#13184,#13185,#13186,
#13187,#13188));
#13808=CLOSED_SHELL('',(#13189,#13190,#13191,#13192,#13193,#13194,#13195,
#13196,#13197,#13198,#13199,#13200,#13201,#13202,#13203,#13204,#13205,#13206,
#13207,#13208,#13209,#13210,#13211,#13212,#13213,#13214,#13215,#13216,#13217,
#13218,#13219,#13220,#13221,#13222,#13223,#13224,#13225,#13226,#13227,#13228,
#13229,#13230,#13231,#13232,#13233,#13234,#13235,#13236,#13237,#13238,#13239,
#13240,#13241,#13242,#13243,#13244,#13245,#13246,#13247,#13248,#13249,#13250,
#13251,#13252,#13253,#13254,#13255,#13256,#13257,#13258,#13259,#13260,#13261,
#13262,#13263,#13264,#13265,#13266,#13267,#13268,#13269,#13270,#13271,#13272,
#13273,#13274,#13275,#13276,#13277));
#13809=CLOSED_SHELL('',(#13278,#13279,#13280,#13281,#13282,#13283,#13284,
#13285,#13286,#13287,#13288,#13289,#13290,#13291,#13292,#13293,#13294,#13295,
#13296,#13297,#13298,#13299,#13300,#13301,#13302,#13303,#13304,#13305,#13306,
#13307,#13308,#13309,#13310,#13311,#13312,#13313,#13314,#13315,#13316,#13317,
#13318,#13319,#13320,#13321,#13322,#13323));
#13810=CLOSED_SHELL('',(#13324,#13325,#13326,#13327,#13328,#13329,#13330,
#13331,#13332,#13333,#13334,#13335,#13336,#13337,#13338,#13339,#13340,#13341,
#13342,#13343,#13344,#13345,#13346,#13347,#13348,#13349,#13350,#13351,#13352,
#13353,#13354,#13355,#13356,#13357));
#13811=CLOSED_SHELL('',(#13358,#13359,#13360,#13361,#13362,#13363,#13364,
#13365,#13366,#13367,#13368,#13369,#13370,#13371,#13372,#13373,#13374,#13375,
#13376,#13377,#13378,#13379,#13380,#13381,#13382,#13383,#13384,#13385,#13386,
#13387,#13388,#13389,#13390,#13391,#13392,#13393,#13394,#13395,#13396,#13397,
#13398,#13399,#13400,#13401,#13402,#13403,#13404,#13405,#13406,#13407,#13408,
#13409,#13410,#13411,#13412,#13413,#13414,#13415,#13416,#13417,#13418,#13419,
#13420,#13421,#13422,#13423,#13424,#13425,#13426,#13427,#13428,#13429,#13430,
#13431,#13432,#13433,#13434,#13435,#13436,#13437,#13438,#13439,#13440,#13441,
#13442,#13443,#13444,#13445,#13446,#13447,#13448,#13449,#13450,#13451,#13452,
#13453,#13454,#13455,#13456,#13457,#13458,#13459,#13460,#13461,#13462,#13463,
#13464,#13465,#13466,#13467,#13468,#13469,#13470,#13471,#13472,#13473));
#13812=CLOSED_SHELL('',(#13474,#13475,#13476,#13477,#13478,#13479,#13480));
#13813=CLOSED_SHELL('',(#13481,#13482,#13483,#13484,#13485));
#13814=CLOSED_SHELL('',(#13486,#13487,#13488,#13489,#13490,#13491,#13492,
#13493,#13494,#13495,#13496,#13497,#13498,#13499,#13500,#13501,#13502,#13503,
#13504,#13505,#13506,#13507,#13508,#13509,#13510,#13511,#13512,#13513,#13514,
#13515,#13516,#13517,#13518,#13519,#13520,#13521,#13522,#13523,#13524,#13525,
#13526,#13527,#13528,#13529,#13530,#13531,#13532,#13533,#13534,#13535,#13536,
#13537));
#13815=CLOSED_SHELL('',(#13538,#13539,#13540,#13541,#13542,#13543,#13544,
#13545,#13546,#13547,#13548,#13549,#13550,#13551,#13552,#13553,#13554,#13555,
#13556,#13557,#13558,#13559,#13560,#13561,#13562,#13563,#13564,#13565,#13566,
#13567,#13568,#13569,#13570,#13571,#13572,#13573,#13574,#13575,#13576,#13577,
#13578,#13579,#13580,#13581,#13582,#13583,#13584,#13585,#13586,#13587,#13588,
#13589,#13590,#13591,#13592,#13593,#13594,#13595,#13596,#13597,#13598,#13599,
#13600,#13601,#13602,#13603,#13604,#13605,#13606,#13607,#13608,#13609,#13610,
#13611,#13612,#13613,#13614,#13615,#13616,#13617,#13618,#13619,#13620,#13621,
#13622,#13623,#13624,#13625,#13626,#13627,#13628));
#13816=CLOSED_SHELL('',(#13629,#13630,#13631,#13632,#13633,#13634,#13635,
#13636,#13637,#13638,#13639,#13640,#13641,#13642,#13643,#13644,#13645,#13646,
#13647,#13648,#13649,#13650,#13651,#13652,#13653,#13654,#13655,#13656,#13657,
#13658,#13659,#13660,#13661,#13662,#13663,#13664,#13665,#13666,#13667,#13668,
#13669,#13670,#13671,#13672,#13673,#13674,#13675,#13676,#13677,#13678,#13679,
#13680,#13681,#13682,#13683,#13684,#13685,#13686,#13687,#13688,#13689,#13690,
#13691,#13692,#13693,#13694,#13695,#13696,#13697,#13698,#13699,#13700,#13701,
#13702,#13703,#13704,#13705,#13706,#13707,#13708,#13709,#13710));
#13817=CLOSED_SHELL('',(#13711,#13712,#13713,#13714,#13715,#13716,#13717,
#13718,#13719,#13720,#13721,#13722,#13723,#13724,#13725,#13726,#13727,#13728,
#13729,#13730,#13731,#13732,#13733,#13734,#13735,#13736,#13737,#13738,#13739,
#13740,#13741,#13742,#13743,#13744,#13745,#13746,#13747,#13748,#13749,#13750,
#13751,#13752,#13753,#13754,#13755,#13756,#13757,#13758,#13759,#13760,#13761,
#13762,#13763,#13764,#13765,#13766,#13767,#13768,#13769,#13770,#13771,#13772,
#13773,#13774,#13775,#13776,#13777,#13778,#13779,#13780,#13781,#13782,#13783,
#13784,#13785,#13786,#13787,#13788,#13789,#13790,#13791,#13792,#13793,#13794,
#13795,#13796,#13797,#13798,#13799,#13800,#13801,#13802,#13803));
#13818=DERIVED_UNIT_ELEMENT(#13846,1.);
#13819=DERIVED_UNIT_ELEMENT(#32311,-3.);
#13820=DERIVED_UNIT_ELEMENT(#13846,1.);
#13821=DERIVED_UNIT_ELEMENT(#32311,-3.);
#13822=DERIVED_UNIT_ELEMENT(#13846,1.);
#13823=DERIVED_UNIT_ELEMENT(#32311,-3.);
#13824=DERIVED_UNIT_ELEMENT(#13846,1.);
#13825=DERIVED_UNIT_ELEMENT(#32311,-3.);
#13826=DERIVED_UNIT_ELEMENT(#13846,1.);
#13827=DERIVED_UNIT_ELEMENT(#32311,-3.);
#13828=DERIVED_UNIT_ELEMENT(#13846,1.);
#13829=DERIVED_UNIT_ELEMENT(#32311,-3.);
#13830=DERIVED_UNIT_ELEMENT(#13846,1.);
#13831=DERIVED_UNIT_ELEMENT(#32311,-3.);
#13832=DERIVED_UNIT_ELEMENT(#13846,1.);
#13833=DERIVED_UNIT_ELEMENT(#32311,-3.);
#13834=DERIVED_UNIT_ELEMENT(#13846,1.);
#13835=DERIVED_UNIT_ELEMENT(#32311,-3.);
#13836=DERIVED_UNIT_ELEMENT(#13846,1.);
#13837=DERIVED_UNIT_ELEMENT(#32311,-3.);
#13838=DERIVED_UNIT_ELEMENT(#13846,1.);
#13839=DERIVED_UNIT_ELEMENT(#32311,-3.);
#13840=DERIVED_UNIT_ELEMENT(#13846,1.);
#13841=DERIVED_UNIT_ELEMENT(#32311,-3.);
#13842=DERIVED_UNIT_ELEMENT(#13846,1.);
#13843=DERIVED_UNIT_ELEMENT(#32311,-3.);
#13844=DERIVED_UNIT_ELEMENT(#13846,1.);
#13845=DERIVED_UNIT_ELEMENT(#32311,-3.);
#13846=(
MASS_UNIT()
NAMED_UNIT(*)
SI_UNIT(.KILO.,.GRAM.)
);
#13847=DERIVED_UNIT((#13818,#13819));
#13848=DERIVED_UNIT((#13820,#13821));
#13849=DERIVED_UNIT((#13822,#13823));
#13850=DERIVED_UNIT((#13824,#13825));
#13851=DERIVED_UNIT((#13826,#13827));
#13852=DERIVED_UNIT((#13828,#13829));
#13853=DERIVED_UNIT((#13830,#13831));
#13854=DERIVED_UNIT((#13832,#13833));
#13855=DERIVED_UNIT((#13834,#13835));
#13856=DERIVED_UNIT((#13836,#13837));
#13857=DERIVED_UNIT((#13838,#13839));
#13858=DERIVED_UNIT((#13840,#13841));
#13859=DERIVED_UNIT((#13842,#13843));
#13860=DERIVED_UNIT((#13844,#13845));
#13861=MEASURE_REPRESENTATION_ITEM('density measure',
POSITIVE_RATIO_MEASURE(7850.),#13847);
#13862=MEASURE_REPRESENTATION_ITEM('density measure',
POSITIVE_RATIO_MEASURE(7850.),#13848);
#13863=MEASURE_REPRESENTATION_ITEM('density measure',
POSITIVE_RATIO_MEASURE(7850.),#13849);
#13864=MEASURE_REPRESENTATION_ITEM('density measure',
POSITIVE_RATIO_MEASURE(7850.),#13850);
#13865=MEASURE_REPRESENTATION_ITEM('density measure',
POSITIVE_RATIO_MEASURE(7850.),#13851);
#13866=MEASURE_REPRESENTATION_ITEM('density measure',
POSITIVE_RATIO_MEASURE(7850.),#13852);
#13867=MEASURE_REPRESENTATION_ITEM('density measure',
POSITIVE_RATIO_MEASURE(7850.),#13853);
#13868=MEASURE_REPRESENTATION_ITEM('density measure',
POSITIVE_RATIO_MEASURE(7850.),#13854);
#13869=MEASURE_REPRESENTATION_ITEM('density measure',
POSITIVE_RATIO_MEASURE(7850.),#13855);
#13870=MEASURE_REPRESENTATION_ITEM('density measure',
POSITIVE_RATIO_MEASURE(7850.),#13856);
#13871=MEASURE_REPRESENTATION_ITEM('density measure',
POSITIVE_RATIO_MEASURE(7850.),#13857);
#13872=MEASURE_REPRESENTATION_ITEM('density measure',
POSITIVE_RATIO_MEASURE(7850.),#13858);
#13873=MEASURE_REPRESENTATION_ITEM('density measure',
POSITIVE_RATIO_MEASURE(7850.),#13859);
#13874=MEASURE_REPRESENTATION_ITEM('density measure',
POSITIVE_RATIO_MEASURE(7850.),#13860);
#13875=PROPERTY_DEFINITION_REPRESENTATION(#13945,#13903);
#13876=PROPERTY_DEFINITION_REPRESENTATION(#13946,#13904);
#13877=PROPERTY_DEFINITION_REPRESENTATION(#13947,#13905);
#13878=PROPERTY_DEFINITION_REPRESENTATION(#13948,#13906);
#13879=PROPERTY_DEFINITION_REPRESENTATION(#13949,#13907);
#13880=PROPERTY_DEFINITION_REPRESENTATION(#13950,#13908);
#13881=PROPERTY_DEFINITION_REPRESENTATION(#13951,#13909);
#13882=PROPERTY_DEFINITION_REPRESENTATION(#13952,#13910);
#13883=PROPERTY_DEFINITION_REPRESENTATION(#13953,#13911);
#13884=PROPERTY_DEFINITION_REPRESENTATION(#13954,#13912);
#13885=PROPERTY_DEFINITION_REPRESENTATION(#13955,#13913);
#13886=PROPERTY_DEFINITION_REPRESENTATION(#13956,#13914);
#13887=PROPERTY_DEFINITION_REPRESENTATION(#13957,#13915);
#13888=PROPERTY_DEFINITION_REPRESENTATION(#13958,#13916);
#13889=PROPERTY_DEFINITION_REPRESENTATION(#13959,#13917);
#13890=PROPERTY_DEFINITION_REPRESENTATION(#13960,#13918);
#13891=PROPERTY_DEFINITION_REPRESENTATION(#13961,#13919);
#13892=PROPERTY_DEFINITION_REPRESENTATION(#13962,#13920);
#13893=PROPERTY_DEFINITION_REPRESENTATION(#13963,#13921);
#13894=PROPERTY_DEFINITION_REPRESENTATION(#13964,#13922);
#13895=PROPERTY_DEFINITION_REPRESENTATION(#13965,#13923);
#13896=PROPERTY_DEFINITION_REPRESENTATION(#13966,#13924);
#13897=PROPERTY_DEFINITION_REPRESENTATION(#13967,#13925);
#13898=PROPERTY_DEFINITION_REPRESENTATION(#13968,#13926);
#13899=PROPERTY_DEFINITION_REPRESENTATION(#13969,#13927);
#13900=PROPERTY_DEFINITION_REPRESENTATION(#13970,#13928);
#13901=PROPERTY_DEFINITION_REPRESENTATION(#13971,#13929);
#13902=PROPERTY_DEFINITION_REPRESENTATION(#13972,#13930);
#13903=REPRESENTATION('material name',(#13931),#32295);
#13904=REPRESENTATION('density',(#13861),#32295);
#13905=REPRESENTATION('material name',(#13932),#32296);
#13906=REPRESENTATION('density',(#13862),#32296);
#13907=REPRESENTATION('material name',(#13933),#32297);
#13908=REPRESENTATION('density',(#13863),#32297);
#13909=REPRESENTATION('material name',(#13934),#32298);
#13910=REPRESENTATION('density',(#13864),#32298);
#13911=REPRESENTATION('material name',(#13935),#32299);
#13912=REPRESENTATION('density',(#13865),#32299);
#13913=REPRESENTATION('material name',(#13936),#32300);
#13914=REPRESENTATION('density',(#13866),#32300);
#13915=REPRESENTATION('material name',(#13937),#32301);
#13916=REPRESENTATION('density',(#13867),#32301);
#13917=REPRESENTATION('material name',(#13938),#32302);
#13918=REPRESENTATION('density',(#13868),#32302);
#13919=REPRESENTATION('material name',(#13939),#32303);
#13920=REPRESENTATION('density',(#13869),#32303);
#13921=REPRESENTATION('material name',(#13940),#32304);
#13922=REPRESENTATION('density',(#13870),#32304);
#13923=REPRESENTATION('material name',(#13941),#32305);
#13924=REPRESENTATION('density',(#13871),#32305);
#13925=REPRESENTATION('material name',(#13942),#32306);
#13926=REPRESENTATION('density',(#13872),#32306);
#13927=REPRESENTATION('material name',(#13943),#32307);
#13928=REPRESENTATION('density',(#13873),#32307);
#13929=REPRESENTATION('material name',(#13944),#32308);
#13930=REPRESENTATION('density',(#13874),#32308);
#13931=DESCRIPTIVE_REPRESENTATION_ITEM('Steel','Steel');
#13932=DESCRIPTIVE_REPRESENTATION_ITEM('Steel','Steel');
#13933=DESCRIPTIVE_REPRESENTATION_ITEM('Steel','Steel');
#13934=DESCRIPTIVE_REPRESENTATION_ITEM('Steel','Steel');
#13935=DESCRIPTIVE_REPRESENTATION_ITEM('Steel','Steel');
#13936=DESCRIPTIVE_REPRESENTATION_ITEM('Steel','Steel');
#13937=DESCRIPTIVE_REPRESENTATION_ITEM('Steel','Steel');
#13938=DESCRIPTIVE_REPRESENTATION_ITEM('Steel','Steel');
#13939=DESCRIPTIVE_REPRESENTATION_ITEM('Steel','Steel');
#13940=DESCRIPTIVE_REPRESENTATION_ITEM('Steel','Steel');
#13941=DESCRIPTIVE_REPRESENTATION_ITEM('Steel','Steel');
#13942=DESCRIPTIVE_REPRESENTATION_ITEM('Steel','Steel');
#13943=DESCRIPTIVE_REPRESENTATION_ITEM('Steel','Steel');
#13944=DESCRIPTIVE_REPRESENTATION_ITEM('Steel','Steel');
#13945=PROPERTY_DEFINITION('material property','material name',#32378);
#13946=PROPERTY_DEFINITION('material property','density of part',#32378);
#13947=PROPERTY_DEFINITION('material property','material name',#32379);
#13948=PROPERTY_DEFINITION('material property','density of part',#32379);
#13949=PROPERTY_DEFINITION('material property','material name',#32380);
#13950=PROPERTY_DEFINITION('material property','density of part',#32380);
#13951=PROPERTY_DEFINITION('material property','material name',#32381);
#13952=PROPERTY_DEFINITION('material property','density of part',#32381);
#13953=PROPERTY_DEFINITION('material property','material name',#32382);
#13954=PROPERTY_DEFINITION('material property','density of part',#32382);
#13955=PROPERTY_DEFINITION('material property','material name',#32383);
#13956=PROPERTY_DEFINITION('material property','density of part',#32383);
#13957=PROPERTY_DEFINITION('material property','material name',#32384);
#13958=PROPERTY_DEFINITION('material property','density of part',#32384);
#13959=PROPERTY_DEFINITION('material property','material name',#32385);
#13960=PROPERTY_DEFINITION('material property','density of part',#32385);
#13961=PROPERTY_DEFINITION('material property','material name',#32386);
#13962=PROPERTY_DEFINITION('material property','density of part',#32386);
#13963=PROPERTY_DEFINITION('material property','material name',#32387);
#13964=PROPERTY_DEFINITION('material property','density of part',#32387);
#13965=PROPERTY_DEFINITION('material property','material name',#32388);
#13966=PROPERTY_DEFINITION('material property','density of part',#32388);
#13967=PROPERTY_DEFINITION('material property','material name',#32389);
#13968=PROPERTY_DEFINITION('material property','density of part',#32389);
#13969=PROPERTY_DEFINITION('material property','material name',#32390);
#13970=PROPERTY_DEFINITION('material property','density of part',#32390);
#13971=PROPERTY_DEFINITION('material property','material name',#32391);
#13972=PROPERTY_DEFINITION('material property','density of part',#32391);
#13973=AXIS2_PLACEMENT_3D('',#18377,#15004,#15005);
#13974=AXIS2_PLACEMENT_3D('',#18378,#15006,#15007);
#13975=AXIS2_PLACEMENT_3D('',#18379,#15008,#15009);
#13976=AXIS2_PLACEMENT_3D('',#18388,#15014,#15015);
#13977=AXIS2_PLACEMENT_3D('',#18392,#15017,#15018);
#13978=AXIS2_PLACEMENT_3D('',#18393,#15019,#15020);
#13979=AXIS2_PLACEMENT_3D('',#18394,#15021,#15022);
#13980=AXIS2_PLACEMENT_3D('',#18400,#15026,#15027);
#13981=AXIS2_PLACEMENT_3D('',#18404,#15029,#15030);
#13982=AXIS2_PLACEMENT_3D('',#18405,#15031,#15032);
#13983=AXIS2_PLACEMENT_3D('',#18406,#15033,#15034);
#13984=AXIS2_PLACEMENT_3D('',#18412,#15038,#15039);
#13985=AXIS2_PLACEMENT_3D('',#18416,#15041,#15042);
#13986=AXIS2_PLACEMENT_3D('',#18417,#15043,#15044);
#13987=AXIS2_PLACEMENT_3D('',#18418,#15045,#15046);
#13988=AXIS2_PLACEMENT_3D('',#18424,#15050,#15051);
#13989=AXIS2_PLACEMENT_3D('',#18425,#15052,#15053);
#13990=AXIS2_PLACEMENT_3D('',#18426,#15054,#15055);
#13991=AXIS2_PLACEMENT_3D('',#18427,#15056,#15057);
#13992=AXIS2_PLACEMENT_3D('',#18431,#15059,#15060);
#13993=AXIS2_PLACEMENT_3D('',#18433,#15062,#15063);
#13994=AXIS2_PLACEMENT_3D('',#18438,#15066,#15067);
#13995=AXIS2_PLACEMENT_3D('',#18439,#15068,#15069);
#13996=AXIS2_PLACEMENT_3D('',#18442,#15071,#15072);
#13997=AXIS2_PLACEMENT_3D('',#18443,#15073,#15074);
#13998=AXIS2_PLACEMENT_3D('',#18447,#15077,#15078);
#13999=AXIS2_PLACEMENT_3D('',#18452,#15080,#15081);
#14000=AXIS2_PLACEMENT_3D('',#18456,#15083,#15084);
#14001=AXIS2_PLACEMENT_3D('',#18460,#15086,#15087);
#14002=AXIS2_PLACEMENT_3D('',#18463,#15089,#15090);
#14003=AXIS2_PLACEMENT_3D('',#18464,#15091,#15092);
#14004=AXIS2_PLACEMENT_3D('',#18470,#15096,#15097);
#14005=AXIS2_PLACEMENT_3D('',#18473,#15099,#15100);
#14006=AXIS2_PLACEMENT_3D('',#18474,#15101,#15102);
#14007=AXIS2_PLACEMENT_3D('',#18478,#15105,#15106);
#14008=AXIS2_PLACEMENT_3D('',#18481,#15108,#15109);
#14009=AXIS2_PLACEMENT_3D('',#18482,#15110,#15111);
#14010=AXIS2_PLACEMENT_3D('',#18486,#15114,#15115);
#14011=AXIS2_PLACEMENT_3D('',#18489,#15117,#15118);
#14012=AXIS2_PLACEMENT_3D('',#18490,#15119,#15120);
#14013=AXIS2_PLACEMENT_3D('',#18494,#15123,#15124);
#14014=AXIS2_PLACEMENT_3D('',#18495,#15125,#15126);
#14015=AXIS2_PLACEMENT_3D('',#18496,#15127,#15128);
#14016=AXIS2_PLACEMENT_3D('',#18500,#15130,#15131);
#14017=AXIS2_PLACEMENT_3D('',#18502,#15133,#15134);
#14018=AXIS2_PLACEMENT_3D('',#18506,#15137,#15138);
#14019=AXIS2_PLACEMENT_3D('',#18509,#15140,#15141);
#14020=AXIS2_PLACEMENT_3D('',#18510,#15142,#15143);
#14021=AXIS2_PLACEMENT_3D('',#18514,#15146,#15147);
#14022=AXIS2_PLACEMENT_3D('',#18520,#15151,#15152);
#14023=AXIS2_PLACEMENT_3D('',#18523,#15154,#15155);
#14024=AXIS2_PLACEMENT_3D('',#18524,#15156,#15157);
#14025=AXIS2_PLACEMENT_3D('',#18530,#15161,#15162);
#14026=AXIS2_PLACEMENT_3D('',#18534,#15164,#15165);
#14027=AXIS2_PLACEMENT_3D('',#18535,#15166,#15167);
#14028=AXIS2_PLACEMENT_3D('',#18536,#15168,#15169);
#14029=AXIS2_PLACEMENT_3D('',#18542,#15173,#15174);
#14030=AXIS2_PLACEMENT_3D('',#18545,#15176,#15177);
#14031=AXIS2_PLACEMENT_3D('',#18546,#15178,#15179);
#14032=AXIS2_PLACEMENT_3D('',#18547,#15180,#15181);
#14033=AXIS2_PLACEMENT_3D('',#18551,#15184,#15185);
#14034=AXIS2_PLACEMENT_3D('',#18552,#15186,#15187);
#14035=AXIS2_PLACEMENT_3D('',#18553,#15188,#15189);
#14036=AXIS2_PLACEMENT_3D('',#18555,#15191,#15192);
#14037=AXIS2_PLACEMENT_3D('',#18560,#15194,#15195);
#14038=AXIS2_PLACEMENT_3D('',#18564,#15197,#15198);
#14039=AXIS2_PLACEMENT_3D('',#18568,#15200,#15201);
#14040=AXIS2_PLACEMENT_3D('',#18571,#15203,#15204);
#14041=AXIS2_PLACEMENT_3D('',#18572,#15205,#15206);
#14042=AXIS2_PLACEMENT_3D('',#18575,#15209,#15210);
#14043=AXIS2_PLACEMENT_3D('',#18577,#15212,#15213);
#14044=AXIS2_PLACEMENT_3D('',#18581,#15216,#15217);
#14045=AXIS2_PLACEMENT_3D('',#18584,#15219,#15220);
#14046=AXIS2_PLACEMENT_3D('',#18585,#15221,#15222);
#14047=AXIS2_PLACEMENT_3D('',#18589,#15225,#15226);
#14048=AXIS2_PLACEMENT_3D('',#18591,#15228,#15229);
#14049=AXIS2_PLACEMENT_3D('',#18592,#15230,#15231);
#14050=AXIS2_PLACEMENT_3D('',#18594,#15233,#15234);
#14051=AXIS2_PLACEMENT_3D('',#18595,#15235,#15236);
#14052=AXIS2_PLACEMENT_3D('',#18597,#15238,#15239);
#14053=AXIS2_PLACEMENT_3D('',#18599,#15240,#15241);
#14054=AXIS2_PLACEMENT_3D('',#18601,#15243,#15244);
#14055=AXIS2_PLACEMENT_3D('',#18603,#15246,#15247);
#14056=AXIS2_PLACEMENT_3D('',#18605,#15249,#15250);
#14057=AXIS2_PLACEMENT_3D('',#18606,#15251,#15252);
#14058=AXIS2_PLACEMENT_3D('',#18608,#15254,#15255);
#14059=AXIS2_PLACEMENT_3D('',#18610,#15257,#15258);
#14060=AXIS2_PLACEMENT_3D('',#18611,#15259,#15260);
#14061=AXIS2_PLACEMENT_3D('',#18993,#15264,#15265);
#14062=AXIS2_PLACEMENT_3D('',#18998,#15267,#15268);
#14063=AXIS2_PLACEMENT_3D('',#19001,#15270,#15271);
#14064=AXIS2_PLACEMENT_3D('',#19089,#15273,#15274);
#14065=AXIS2_PLACEMENT_3D('',#19183,#15277,#15278);
#14066=AXIS2_PLACEMENT_3D('',#19195,#15285,#15286);
#14067=AXIS2_PLACEMENT_3D('',#19264,#15288,#15289);
#14068=AXIS2_PLACEMENT_3D('',#19617,#15292,#15293);
#14069=AXIS2_PLACEMENT_3D('',#19622,#15295,#15296);
#14070=AXIS2_PLACEMENT_3D('',#19625,#15298,#15299);
#14071=AXIS2_PLACEMENT_3D('',#19713,#15301,#15302);
#14072=AXIS2_PLACEMENT_3D('',#19717,#15304,#15305);
#14073=AXIS2_PLACEMENT_3D('',#19721,#15307,#15308);
#14074=AXIS2_PLACEMENT_3D('',#20101,#15312,#15313);
#14075=AXIS2_PLACEMENT_3D('',#20106,#15315,#15316);
#14076=AXIS2_PLACEMENT_3D('',#20109,#15318,#15319);
#14077=AXIS2_PLACEMENT_3D('',#20197,#15321,#15322);
#14078=AXIS2_PLACEMENT_3D('',#20289,#15324,#15325);
#14079=AXIS2_PLACEMENT_3D('',#20465,#15329,#15330);
#14080=AXIS2_PLACEMENT_3D('',#20469,#15332,#15333);
#14081=AXIS2_PLACEMENT_3D('',#20543,#15336,#15337);
#14082=AXIS2_PLACEMENT_3D('',#20547,#15339,#15340);
#14083=AXIS2_PLACEMENT_3D('',#20551,#15342,#15343);
#14084=AXIS2_PLACEMENT_3D('',#20553,#15345,#15346);
#14085=AXIS2_PLACEMENT_3D('',#20562,#15348,#15349);
#14086=AXIS2_PLACEMENT_3D('',#20586,#15352,#15353);
#14087=AXIS2_PLACEMENT_3D('',#20588,#15355,#15356);
#14088=AXIS2_PLACEMENT_3D('',#20589,#15357,#15358);
#14089=AXIS2_PLACEMENT_3D('',#20598,#15360,#15361);
#14090=AXIS2_PLACEMENT_3D('',#20622,#15364,#15365);
#14091=AXIS2_PLACEMENT_3D('',#20624,#15367,#15368);
#14092=AXIS2_PLACEMENT_3D('',#20625,#15369,#15370);
#14093=AXIS2_PLACEMENT_3D('',#20627,#15372,#15373);
#14094=AXIS2_PLACEMENT_3D('',#20629,#15375,#15376);
#14095=AXIS2_PLACEMENT_3D('',#20630,#15377,#15378);
#14096=AXIS2_PLACEMENT_3D('',#20926,#15382,#15383);
#14097=AXIS2_PLACEMENT_3D('',#20968,#15387,#15388);
#14098=AXIS2_PLACEMENT_3D('',#21026,#15391,#15392);
#14099=AXIS2_PLACEMENT_3D('',#21030,#15395,#15396);
#14100=AXIS2_PLACEMENT_3D('',#21086,#15398,#15399);
#14101=AXIS2_PLACEMENT_3D('',#21282,#15408,#15409);
#14102=AXIS2_PLACEMENT_3D('',#21316,#15412,#15413);
#14103=AXIS2_PLACEMENT_3D('',#21374,#15416,#15417);
#14104=AXIS2_PLACEMENT_3D('',#21378,#15420,#15421);
#14105=AXIS2_PLACEMENT_3D('',#21616,#15424,#15425);
#14106=AXIS2_PLACEMENT_3D('',#21936,#15430,#15431);
#14107=AXIS2_PLACEMENT_3D('',#21978,#15435,#15436);
#14108=AXIS2_PLACEMENT_3D('',#21980,#15438,#15439);
#14109=AXIS2_PLACEMENT_3D('',#21982,#15441,#15442);
#14110=AXIS2_PLACEMENT_3D('',#21984,#15444,#15445);
#14111=AXIS2_PLACEMENT_3D('',#21987,#15448,#15449);
#14112=AXIS2_PLACEMENT_3D('',#21988,#15450,#15451);
#14113=AXIS2_PLACEMENT_3D('',#21990,#15453,#15454);
#14114=AXIS2_PLACEMENT_3D('',#21991,#15455,#15456);
#14115=AXIS2_PLACEMENT_3D('',#21992,#15457,#15458);
#14116=AXIS2_PLACEMENT_3D('',#21994,#15459,#15460);
#14117=AXIS2_PLACEMENT_3D('',#21997,#15462,#15463);
#14118=AXIS2_PLACEMENT_3D('',#21998,#15464,#15465);
#14119=AXIS2_PLACEMENT_3D('',#22001,#15467,#15468);
#14120=AXIS2_PLACEMENT_3D('',#22002,#15469,#15470);
#14121=AXIS2_PLACEMENT_3D('',#22011,#15475,#15476);
#14122=AXIS2_PLACEMENT_3D('',#22013,#15477,#15478);
#14123=AXIS2_PLACEMENT_3D('',#22015,#15480,#15481);
#14124=AXIS2_PLACEMENT_3D('',#22024,#15486,#15487);
#14125=AXIS2_PLACEMENT_3D('',#22033,#15492,#15493);
#14126=AXIS2_PLACEMENT_3D('',#22037,#15495,#15496);
#14127=AXIS2_PLACEMENT_3D('',#22038,#15497,#15498);
#14128=AXIS2_PLACEMENT_3D('',#22039,#15499,#15500);
#14129=AXIS2_PLACEMENT_3D('',#22045,#15504,#15505);
#14130=AXIS2_PLACEMENT_3D('',#22048,#15507,#15508);
#14131=AXIS2_PLACEMENT_3D('',#22049,#15509,#15510);
#14132=AXIS2_PLACEMENT_3D('',#22050,#15511,#15512);
#14133=AXIS2_PLACEMENT_3D('',#22054,#15515,#15516);
#14134=AXIS2_PLACEMENT_3D('',#22058,#15518,#15519);
#14135=AXIS2_PLACEMENT_3D('',#22059,#15520,#15521);
#14136=AXIS2_PLACEMENT_3D('',#22060,#15522,#15523);
#14137=AXIS2_PLACEMENT_3D('',#22066,#15527,#15528);
#14138=AXIS2_PLACEMENT_3D('',#22067,#15529,#15530);
#14139=AXIS2_PLACEMENT_3D('',#22068,#15531,#15532);
#14140=AXIS2_PLACEMENT_3D('',#22069,#15533,#15534);
#14141=AXIS2_PLACEMENT_3D('',#22072,#15536,#15537);
#14142=AXIS2_PLACEMENT_3D('',#22073,#15538,#15539);
#14143=AXIS2_PLACEMENT_3D('',#22077,#15542,#15543);
#14144=AXIS2_PLACEMENT_3D('',#22080,#15545,#15546);
#14145=AXIS2_PLACEMENT_3D('',#22081,#15547,#15548);
#14146=AXIS2_PLACEMENT_3D('',#22085,#15551,#15552);
#14147=AXIS2_PLACEMENT_3D('',#22088,#15553,#15554);
#14148=AXIS2_PLACEMENT_3D('',#22092,#15556,#15557);
#14149=AXIS2_PLACEMENT_3D('',#22096,#15559,#15560);
#14150=AXIS2_PLACEMENT_3D('',#22100,#15562,#15563);
#14151=AXIS2_PLACEMENT_3D('',#22102,#15565,#15566);
#14152=AXIS2_PLACEMENT_3D('',#22106,#15569,#15570);
#14153=AXIS2_PLACEMENT_3D('',#22107,#15571,#15572);
#14154=AXIS2_PLACEMENT_3D('',#22111,#15575,#15576);
#14155=AXIS2_PLACEMENT_3D('',#22114,#15578,#15579);
#14156=AXIS2_PLACEMENT_3D('',#22115,#15580,#15581);
#14157=AXIS2_PLACEMENT_3D('',#22119,#15584,#15585);
#14158=AXIS2_PLACEMENT_3D('',#22122,#15587,#15588);
#14159=AXIS2_PLACEMENT_3D('',#22123,#15589,#15590);
#14160=AXIS2_PLACEMENT_3D('',#22127,#15593,#15594);
#14161=AXIS2_PLACEMENT_3D('',#22129,#15596,#15597);
#14162=AXIS2_PLACEMENT_3D('',#22130,#15598,#15599);
#14163=AXIS2_PLACEMENT_3D('',#22131,#15600,#15601);
#14164=AXIS2_PLACEMENT_3D('',#22137,#15605,#15606);
#14165=AXIS2_PLACEMENT_3D('',#22140,#15608,#15609);
#14166=AXIS2_PLACEMENT_3D('',#22141,#15610,#15611);
#14167=AXIS2_PLACEMENT_3D('',#22145,#15614,#15615);
#14168=AXIS2_PLACEMENT_3D('',#22146,#15616,#15617);
#14169=AXIS2_PLACEMENT_3D('',#22147,#15618,#15619);
#14170=AXIS2_PLACEMENT_3D('',#22153,#15623,#15624);
#14171=AXIS2_PLACEMENT_3D('',#22156,#15626,#15627);
#14172=AXIS2_PLACEMENT_3D('',#22157,#15628,#15629);
#14173=AXIS2_PLACEMENT_3D('',#22161,#15632,#15633);
#14174=AXIS2_PLACEMENT_3D('',#22164,#15635,#15636);
#14175=AXIS2_PLACEMENT_3D('',#22165,#15637,#15638);
#14176=AXIS2_PLACEMENT_3D('',#22169,#15641,#15642);
#14177=AXIS2_PLACEMENT_3D('',#22173,#15644,#15645);
#14178=AXIS2_PLACEMENT_3D('',#22174,#15646,#15647);
#14179=AXIS2_PLACEMENT_3D('',#22175,#15648,#15649);
#14180=AXIS2_PLACEMENT_3D('',#22181,#15653,#15654);
#14181=AXIS2_PLACEMENT_3D('',#22182,#15655,#15656);
#14182=AXIS2_PLACEMENT_3D('',#22183,#15657,#15658);
#14183=AXIS2_PLACEMENT_3D('',#22184,#15659,#15660);
#14184=AXIS2_PLACEMENT_3D('',#22189,#15662,#15663);
#14185=AXIS2_PLACEMENT_3D('',#22193,#15665,#15666);
#14186=AXIS2_PLACEMENT_3D('',#22197,#15668,#15669);
#14187=AXIS2_PLACEMENT_3D('',#22200,#15671,#15672);
#14188=AXIS2_PLACEMENT_3D('',#22201,#15673,#15674);
#14189=AXIS2_PLACEMENT_3D('',#22204,#15677,#15678);
#14190=AXIS2_PLACEMENT_3D('',#22206,#15680,#15681);
#14191=AXIS2_PLACEMENT_3D('',#22208,#15683,#15684);
#14192=AXIS2_PLACEMENT_3D('',#22211,#15686,#15687);
#14193=AXIS2_PLACEMENT_3D('',#22212,#15688,#15689);
#14194=AXIS2_PLACEMENT_3D('',#22216,#15692,#15693);
#14195=AXIS2_PLACEMENT_3D('',#22218,#15695,#15696);
#14196=AXIS2_PLACEMENT_3D('',#22219,#15697,#15698);
#14197=AXIS2_PLACEMENT_3D('',#22221,#15700,#15701);
#14198=AXIS2_PLACEMENT_3D('',#22222,#15702,#15703);
#14199=AXIS2_PLACEMENT_3D('',#22224,#15705,#15706);
#14200=AXIS2_PLACEMENT_3D('',#22226,#15708,#15709);
#14201=AXIS2_PLACEMENT_3D('',#22227,#15710,#15711);
#14202=AXIS2_PLACEMENT_3D('',#22229,#15713,#15714);
#14203=AXIS2_PLACEMENT_3D('',#22231,#15716,#15717);
#14204=AXIS2_PLACEMENT_3D('',#22232,#15718,#15719);
#14205=AXIS2_PLACEMENT_3D('',#22233,#15720,#15721);
#14206=AXIS2_PLACEMENT_3D('',#22235,#15722,#15723);
#14207=AXIS2_PLACEMENT_3D('',#22238,#15725,#15726);
#14208=AXIS2_PLACEMENT_3D('',#22239,#15727,#15728);
#14209=AXIS2_PLACEMENT_3D('',#22249,#15733,#15734);
#14210=AXIS2_PLACEMENT_3D('',#22251,#15735,#15736);
#14211=AXIS2_PLACEMENT_3D('',#22253,#15737,#15738);
#14212=AXIS2_PLACEMENT_3D('',#22255,#15739,#15740);
#14213=AXIS2_PLACEMENT_3D('',#22257,#15741,#15742);
#14214=AXIS2_PLACEMENT_3D('',#22258,#15743,#15744);
#14215=AXIS2_PLACEMENT_3D('',#22260,#15745,#15746);
#14216=AXIS2_PLACEMENT_3D('',#22262,#15748,#15749);
#14217=AXIS2_PLACEMENT_3D('',#22265,#15751,#15752);
#14218=AXIS2_PLACEMENT_3D('',#22266,#15753,#15754);
#14219=AXIS2_PLACEMENT_3D('',#22268,#15755,#15756);
#14220=AXIS2_PLACEMENT_3D('',#22270,#15758,#15759);
#14221=AXIS2_PLACEMENT_3D('',#22273,#15761,#15762);
#14222=AXIS2_PLACEMENT_3D('',#22274,#15763,#15764);
#14223=AXIS2_PLACEMENT_3D('',#22276,#15765,#15766);
#14224=AXIS2_PLACEMENT_3D('',#22278,#15768,#15769);
#14225=AXIS2_PLACEMENT_3D('',#22281,#15771,#15772);
#14226=AXIS2_PLACEMENT_3D('',#22282,#15773,#15774);
#14227=AXIS2_PLACEMENT_3D('',#22284,#15775,#15776);
#14228=AXIS2_PLACEMENT_3D('',#22286,#15778,#15779);
#14229=AXIS2_PLACEMENT_3D('',#22289,#15781,#15782);
#14230=AXIS2_PLACEMENT_3D('',#22290,#15783,#15784);
#14231=AXIS2_PLACEMENT_3D('',#22292,#15785,#15786);
#14232=AXIS2_PLACEMENT_3D('',#22294,#15788,#15789);
#14233=AXIS2_PLACEMENT_3D('',#22297,#15791,#15792);
#14234=AXIS2_PLACEMENT_3D('',#22298,#15793,#15794);
#14235=AXIS2_PLACEMENT_3D('',#22300,#15795,#15796);
#14236=AXIS2_PLACEMENT_3D('',#22302,#15798,#15799);
#14237=AXIS2_PLACEMENT_3D('',#22304,#15800,#15801);
#14238=AXIS2_PLACEMENT_3D('',#22307,#15803,#15804);
#14239=AXIS2_PLACEMENT_3D('',#22308,#15805,#15806);
#14240=AXIS2_PLACEMENT_3D('',#22318,#15811,#15812);
#14241=AXIS2_PLACEMENT_3D('',#22320,#15813,#15814);
#14242=AXIS2_PLACEMENT_3D('',#22322,#15815,#15816);
#14243=AXIS2_PLACEMENT_3D('',#22324,#15817,#15818);
#14244=AXIS2_PLACEMENT_3D('',#22326,#15819,#15820);
#14245=AXIS2_PLACEMENT_3D('',#22328,#15821,#15822);
#14246=AXIS2_PLACEMENT_3D('',#22329,#15823,#15824);
#14247=AXIS2_PLACEMENT_3D('',#22331,#15825,#15826);
#14248=AXIS2_PLACEMENT_3D('',#22333,#15828,#15829);
#14249=AXIS2_PLACEMENT_3D('',#22339,#15833,#15834);
#14250=AXIS2_PLACEMENT_3D('',#22343,#15836,#15837);
#14251=AXIS2_PLACEMENT_3D('',#22344,#15838,#15839);
#14252=AXIS2_PLACEMENT_3D('',#22345,#15840,#15841);
#14253=AXIS2_PLACEMENT_3D('',#22351,#15845,#15846);
#14254=AXIS2_PLACEMENT_3D('',#22355,#15848,#15849);
#14255=AXIS2_PLACEMENT_3D('',#22356,#15850,#15851);
#14256=AXIS2_PLACEMENT_3D('',#22357,#15852,#15853);
#14257=AXIS2_PLACEMENT_3D('',#22363,#15857,#15858);
#14258=AXIS2_PLACEMENT_3D('',#22366,#15860,#15861);
#14259=AXIS2_PLACEMENT_3D('',#22367,#15862,#15863);
#14260=AXIS2_PLACEMENT_3D('',#22368,#15864,#15865);
#14261=AXIS2_PLACEMENT_3D('',#22372,#15868,#15869);
#14262=AXIS2_PLACEMENT_3D('',#22373,#15870,#15871);
#14263=AXIS2_PLACEMENT_3D('',#22374,#15872,#15873);
#14264=AXIS2_PLACEMENT_3D('',#22375,#15874,#15875);
#14265=AXIS2_PLACEMENT_3D('',#22377,#15876,#15877);
#14266=AXIS2_PLACEMENT_3D('',#22379,#15879,#15880);
#14267=AXIS2_PLACEMENT_3D('',#22380,#15881,#15882);
#14268=AXIS2_PLACEMENT_3D('',#22381,#15883,#15884);
#14269=AXIS2_PLACEMENT_3D('',#22386,#15886,#15887);
#14270=AXIS2_PLACEMENT_3D('',#22390,#15889,#15890);
#14271=AXIS2_PLACEMENT_3D('',#22394,#15892,#15893);
#14272=AXIS2_PLACEMENT_3D('',#22397,#15895,#15896);
#14273=AXIS2_PLACEMENT_3D('',#22398,#15897,#15898);
#14274=AXIS2_PLACEMENT_3D('',#22401,#15900,#15901);
#14275=AXIS2_PLACEMENT_3D('',#22402,#15902,#15903);
#14276=AXIS2_PLACEMENT_3D('',#22404,#15904,#15905);
#14277=AXIS2_PLACEMENT_3D('',#22406,#15907,#15908);
#14278=AXIS2_PLACEMENT_3D('',#22409,#15910,#15911);
#14279=AXIS2_PLACEMENT_3D('',#22410,#15912,#15913);
#14280=AXIS2_PLACEMENT_3D('',#22412,#15914,#15915);
#14281=AXIS2_PLACEMENT_3D('',#22414,#15917,#15918);
#14282=AXIS2_PLACEMENT_3D('',#22417,#15920,#15921);
#14283=AXIS2_PLACEMENT_3D('',#22418,#15922,#15923);
#14284=AXIS2_PLACEMENT_3D('',#22420,#15924,#15925);
#14285=AXIS2_PLACEMENT_3D('',#22422,#15927,#15928);
#14286=AXIS2_PLACEMENT_3D('',#22425,#15930,#15931);
#14287=AXIS2_PLACEMENT_3D('',#22426,#15932,#15933);
#14288=AXIS2_PLACEMENT_3D('',#22428,#15934,#15935);
#14289=AXIS2_PLACEMENT_3D('',#22430,#15937,#15938);
#14290=AXIS2_PLACEMENT_3D('',#22433,#15940,#15941);
#14291=AXIS2_PLACEMENT_3D('',#22434,#15942,#15943);
#14292=AXIS2_PLACEMENT_3D('',#22436,#15944,#15945);
#14293=AXIS2_PLACEMENT_3D('',#22438,#15947,#15948);
#14294=AXIS2_PLACEMENT_3D('',#22441,#15950,#15951);
#14295=AXIS2_PLACEMENT_3D('',#22442,#15952,#15953);
#14296=AXIS2_PLACEMENT_3D('',#22444,#15954,#15955);
#14297=AXIS2_PLACEMENT_3D('',#22446,#15957,#15958);
#14298=AXIS2_PLACEMENT_3D('',#22448,#15959,#15960);
#14299=AXIS2_PLACEMENT_3D('',#22450,#15962,#15963);
#14300=AXIS2_PLACEMENT_3D('',#22460,#15968,#15969);
#14301=AXIS2_PLACEMENT_3D('',#22462,#15970,#15971);
#14302=AXIS2_PLACEMENT_3D('',#22464,#15972,#15973);
#14303=AXIS2_PLACEMENT_3D('',#22466,#15974,#15975);
#14304=AXIS2_PLACEMENT_3D('',#22468,#15976,#15977);
#14305=AXIS2_PLACEMENT_3D('',#22470,#15978,#15979);
#14306=AXIS2_PLACEMENT_3D('',#22471,#15980,#15981);
#14307=AXIS2_PLACEMENT_3D('',#22473,#15983,#15984);
#14308=AXIS2_PLACEMENT_3D('',#22475,#15986,#15987);
#14309=AXIS2_PLACEMENT_3D('',#22477,#15989,#15990);
#14310=AXIS2_PLACEMENT_3D('',#22479,#15992,#15993);
#14311=AXIS2_PLACEMENT_3D('',#22481,#15995,#15996);
#14312=AXIS2_PLACEMENT_3D('',#22483,#15998,#15999);
#14313=AXIS2_PLACEMENT_3D('',#22489,#16003,#16004);
#14314=AXIS2_PLACEMENT_3D('',#22492,#16006,#16007);
#14315=AXIS2_PLACEMENT_3D('',#22493,#16008,#16009);
#14316=AXIS2_PLACEMENT_3D('',#22497,#16012,#16013);
#14317=AXIS2_PLACEMENT_3D('',#22500,#16015,#16016);
#14318=AXIS2_PLACEMENT_3D('',#22501,#16017,#16018);
#14319=AXIS2_PLACEMENT_3D('',#22505,#16021,#16022);
#14320=AXIS2_PLACEMENT_3D('',#22507,#16024,#16025);
#14321=AXIS2_PLACEMENT_3D('',#22508,#16026,#16027);
#14322=AXIS2_PLACEMENT_3D('',#22510,#16029,#16030);
#14323=AXIS2_PLACEMENT_3D('',#22511,#16031,#16032);
#14324=AXIS2_PLACEMENT_3D('',#22512,#16033,#16034);
#14325=AXIS2_PLACEMENT_3D('',#22514,#16035,#16036);
#14326=AXIS2_PLACEMENT_3D('',#22516,#16038,#16039);
#14327=AXIS2_PLACEMENT_3D('',#22519,#16041,#16042);
#14328=AXIS2_PLACEMENT_3D('',#22520,#16043,#16044);
#14329=AXIS2_PLACEMENT_3D('',#22525,#16047,#16048);
#14330=AXIS2_PLACEMENT_3D('',#22527,#16049,#16050);
#14331=AXIS2_PLACEMENT_3D('',#22529,#16051,#16052);
#14332=AXIS2_PLACEMENT_3D('',#22531,#16053,#16054);
#14333=AXIS2_PLACEMENT_3D('',#22533,#16055,#16056);
#14334=AXIS2_PLACEMENT_3D('',#22535,#16057,#16058);
#14335=AXIS2_PLACEMENT_3D('',#22536,#16059,#16060);
#14336=AXIS2_PLACEMENT_3D('',#22538,#16062,#16063);
#14337=AXIS2_PLACEMENT_3D('',#22540,#16065,#16066);
#14338=AXIS2_PLACEMENT_3D('',#22542,#16068,#16069);
#14339=AXIS2_PLACEMENT_3D('',#22544,#16071,#16072);
#14340=AXIS2_PLACEMENT_3D('',#22546,#16074,#16075);
#14341=AXIS2_PLACEMENT_3D('',#22548,#16077,#16078);
#14342=AXIS2_PLACEMENT_3D('',#22554,#16082,#16083);
#14343=AXIS2_PLACEMENT_3D('',#22557,#16085,#16086);
#14344=AXIS2_PLACEMENT_3D('',#22558,#16087,#16088);
#14345=AXIS2_PLACEMENT_3D('',#22562,#16091,#16092);
#14346=AXIS2_PLACEMENT_3D('',#22566,#16094,#16095);
#14347=AXIS2_PLACEMENT_3D('',#22567,#16096,#16097);
#14348=AXIS2_PLACEMENT_3D('',#22568,#16098,#16099);
#14349=AXIS2_PLACEMENT_3D('',#22574,#16103,#16104);
#14350=AXIS2_PLACEMENT_3D('',#22578,#16106,#16107);
#14351=AXIS2_PLACEMENT_3D('',#22579,#16108,#16109);
#14352=AXIS2_PLACEMENT_3D('',#22580,#16110,#16111);
#14353=AXIS2_PLACEMENT_3D('',#22585,#16115,#16116);
#14354=AXIS2_PLACEMENT_3D('',#22586,#16117,#16118);
#14355=AXIS2_PLACEMENT_3D('',#22587,#16119,#16120);
#14356=AXIS2_PLACEMENT_3D('',#22589,#16122,#16123);
#14357=AXIS2_PLACEMENT_3D('',#22594,#16125,#16126);
#14358=AXIS2_PLACEMENT_3D('',#22598,#16128,#16129);
#14359=AXIS2_PLACEMENT_3D('',#22602,#16131,#16132);
#14360=AXIS2_PLACEMENT_3D('',#22605,#16134,#16135);
#14361=AXIS2_PLACEMENT_3D('',#22606,#16136,#16137);
#14362=AXIS2_PLACEMENT_3D('',#22609,#16140,#16141);
#14363=AXIS2_PLACEMENT_3D('',#22611,#16143,#16144);
#14364=AXIS2_PLACEMENT_3D('',#22613,#16146,#16147);
#14365=AXIS2_PLACEMENT_3D('',#22616,#16149,#16150);
#14366=AXIS2_PLACEMENT_3D('',#22617,#16151,#16152);
#14367=AXIS2_PLACEMENT_3D('',#22621,#16155,#16156);
#14368=AXIS2_PLACEMENT_3D('',#22624,#16158,#16159);
#14369=AXIS2_PLACEMENT_3D('',#22625,#16160,#16161);
#14370=AXIS2_PLACEMENT_3D('',#22628,#16164,#16165);
#14371=AXIS2_PLACEMENT_3D('',#22629,#16166,#16167);
#14372=AXIS2_PLACEMENT_3D('',#22631,#16169,#16170);
#14373=AXIS2_PLACEMENT_3D('',#22633,#16172,#16173);
#14374=AXIS2_PLACEMENT_3D('',#22635,#16175,#16176);
#14375=AXIS2_PLACEMENT_3D('',#22636,#16177,#16178);
#14376=AXIS2_PLACEMENT_3D('',#22638,#16180,#16181);
#14377=AXIS2_PLACEMENT_3D('',#22640,#16183,#16184);
#14378=AXIS2_PLACEMENT_3D('',#22641,#16185,#16186);
#14379=AXIS2_PLACEMENT_3D('',#23011,#16190,#16191);
#14380=AXIS2_PLACEMENT_3D('',#23016,#16193,#16194);
#14381=AXIS2_PLACEMENT_3D('',#23019,#16196,#16197);
#14382=AXIS2_PLACEMENT_3D('',#23107,#16199,#16200);
#14383=AXIS2_PLACEMENT_3D('',#23118,#16203,#16204);
#14384=AXIS2_PLACEMENT_3D('',#23126,#16209,#16210);
#14385=AXIS2_PLACEMENT_3D('',#23193,#16212,#16213);
#14386=AXIS2_PLACEMENT_3D('',#23625,#16217,#16218);
#14387=AXIS2_PLACEMENT_3D('',#23630,#16220,#16221);
#14388=AXIS2_PLACEMENT_3D('',#23633,#16223,#16224);
#14389=AXIS2_PLACEMENT_3D('',#23709,#16226,#16227);
#14390=AXIS2_PLACEMENT_3D('',#23719,#16233,#16234);
#14391=AXIS2_PLACEMENT_3D('',#23728,#16236,#16237);
#14392=AXIS2_PLACEMENT_3D('',#23730,#16238,#16239);
#14393=AXIS2_PLACEMENT_3D('',#23733,#16241,#16242);
#14394=AXIS2_PLACEMENT_3D('',#23989,#16246,#16247);
#14395=AXIS2_PLACEMENT_3D('',#23993,#16249,#16250);
#14396=AXIS2_PLACEMENT_3D('',#24057,#16253,#16254);
#14397=AXIS2_PLACEMENT_3D('',#24149,#16257,#16258);
#14398=AXIS2_PLACEMENT_3D('',#24429,#16263,#16264);
#14399=AXIS2_PLACEMENT_3D('',#24434,#16266,#16267);
#14400=AXIS2_PLACEMENT_3D('',#24437,#16269,#16270);
#14401=AXIS2_PLACEMENT_3D('',#24513,#16272,#16273);
#14402=AXIS2_PLACEMENT_3D('',#24517,#16275,#16276);
#14403=AXIS2_PLACEMENT_3D('',#24521,#16278,#16279);
#14404=AXIS2_PLACEMENT_3D('',#24523,#16281,#16282);
#14405=AXIS2_PLACEMENT_3D('',#24524,#16283,#16284);
#14406=AXIS2_PLACEMENT_3D('',#24525,#16285,#16286);
#14407=AXIS2_PLACEMENT_3D('',#24532,#16287,#16288);
#14408=AXIS2_PLACEMENT_3D('',#24548,#16290,#16291);
#14409=AXIS2_PLACEMENT_3D('',#24557,#16293,#16294);
#14410=AXIS2_PLACEMENT_3D('',#24572,#16296,#16297);
#14411=AXIS2_PLACEMENT_3D('',#24574,#16299,#16300);
#14412=AXIS2_PLACEMENT_3D('',#24575,#16301,#16302);
#14413=AXIS2_PLACEMENT_3D('',#24576,#16303,#16304);
#14414=AXIS2_PLACEMENT_3D('',#24866,#16308,#16309);
#14415=AXIS2_PLACEMENT_3D('',#24914,#16313,#16314);
#14416=AXIS2_PLACEMENT_3D('',#24928,#16322,#16323);
#14417=AXIS2_PLACEMENT_3D('',#24984,#16325,#16326);
#14418=AXIS2_PLACEMENT_3D('',#24988,#16329,#16330);
#14419=AXIS2_PLACEMENT_3D('',#25228,#16334,#16335);
#14420=AXIS2_PLACEMENT_3D('',#25548,#16340,#16341);
#14421=AXIS2_PLACEMENT_3D('',#25590,#16345,#16346);
#14422=AXIS2_PLACEMENT_3D('',#25646,#16348,#16349);
#14423=AXIS2_PLACEMENT_3D('',#25650,#16352,#16353);
#14424=AXIS2_PLACEMENT_3D('',#25706,#16355,#16356);
#14425=AXIS2_PLACEMENT_3D('',#25893,#16361,#16362);
#14426=AXIS2_PLACEMENT_3D('',#25927,#16365,#16366);
#14427=AXIS2_PLACEMENT_3D('',#25929,#16368,#16369);
#14428=AXIS2_PLACEMENT_3D('',#25931,#16371,#16372);
#14429=AXIS2_PLACEMENT_3D('',#25932,#16373,#16374);
#14430=AXIS2_PLACEMENT_3D('',#25934,#16376,#16377);
#14431=AXIS2_PLACEMENT_3D('',#25936,#16379,#16380);
#14432=AXIS2_PLACEMENT_3D('',#25937,#16381,#16382);
#14433=AXIS2_PLACEMENT_3D('',#25938,#16383,#16384);
#14434=AXIS2_PLACEMENT_3D('',#25945,#16385,#16386);
#14435=AXIS2_PLACEMENT_3D('',#25948,#16388,#16389);
#14436=AXIS2_PLACEMENT_3D('',#25949,#16390,#16391);
#14437=AXIS2_PLACEMENT_3D('',#25955,#16395,#16396);
#14438=AXIS2_PLACEMENT_3D('',#25961,#16397,#16398);
#14439=AXIS2_PLACEMENT_3D('',#25962,#16399,#16400);
#14440=AXIS2_PLACEMENT_3D('',#25963,#16401,#16402);
#14441=AXIS2_PLACEMENT_3D('',#25969,#16405,#16406);
#14442=AXIS2_PLACEMENT_3D('',#25973,#16408,#16409);
#14443=AXIS2_PLACEMENT_3D('',#25974,#16410,#16411);
#14444=AXIS2_PLACEMENT_3D('',#25975,#16412,#16413);
#14445=AXIS2_PLACEMENT_3D('',#25980,#16416,#16417);
#14446=AXIS2_PLACEMENT_3D('',#25981,#16418,#16419);
#14447=AXIS2_PLACEMENT_3D('',#25985,#16421,#16422);
#14448=AXIS2_PLACEMENT_3D('',#25987,#16423,#16424);
#14449=AXIS2_PLACEMENT_3D('',#25990,#16426,#16427);
#14450=AXIS2_PLACEMENT_3D('',#25991,#16428,#16429);
#14451=AXIS2_PLACEMENT_3D('',#25993,#16430,#16431);
#14452=AXIS2_PLACEMENT_3D('',#25996,#16433,#16434);
#14453=AXIS2_PLACEMENT_3D('',#25997,#16435,#16436);
#14454=AXIS2_PLACEMENT_3D('',#26000,#16437,#16438);
#14455=AXIS2_PLACEMENT_3D('',#26004,#16440,#16441);
#14456=AXIS2_PLACEMENT_3D('',#26008,#16443,#16444);
#14457=AXIS2_PLACEMENT_3D('',#26012,#16446,#16447);
#14458=AXIS2_PLACEMENT_3D('',#26014,#16449,#16450);
#14459=AXIS2_PLACEMENT_3D('',#26017,#16452,#16453);
#14460=AXIS2_PLACEMENT_3D('',#26018,#16454,#16455);
#14461=AXIS2_PLACEMENT_3D('',#26025,#16456,#16457);
#14462=AXIS2_PLACEMENT_3D('',#26028,#16459,#16460);
#14463=AXIS2_PLACEMENT_3D('',#26029,#16461,#16462);
#14464=AXIS2_PLACEMENT_3D('',#26035,#16466,#16467);
#14465=AXIS2_PLACEMENT_3D('',#26041,#16468,#16469);
#14466=AXIS2_PLACEMENT_3D('',#26042,#16470,#16471);
#14467=AXIS2_PLACEMENT_3D('',#26043,#16472,#16473);
#14468=AXIS2_PLACEMENT_3D('',#26049,#16476,#16477);
#14469=AXIS2_PLACEMENT_3D('',#26053,#16479,#16480);
#14470=AXIS2_PLACEMENT_3D('',#26054,#16481,#16482);
#14471=AXIS2_PLACEMENT_3D('',#26055,#16483,#16484);
#14472=AXIS2_PLACEMENT_3D('',#26060,#16487,#16488);
#14473=AXIS2_PLACEMENT_3D('',#26061,#16489,#16490);
#14474=AXIS2_PLACEMENT_3D('',#26065,#16492,#16493);
#14475=AXIS2_PLACEMENT_3D('',#26067,#16494,#16495);
#14476=AXIS2_PLACEMENT_3D('',#26070,#16497,#16498);
#14477=AXIS2_PLACEMENT_3D('',#26071,#16499,#16500);
#14478=AXIS2_PLACEMENT_3D('',#26077,#16504,#16505);
#14479=AXIS2_PLACEMENT_3D('',#26081,#16507,#16508);
#14480=AXIS2_PLACEMENT_3D('',#26082,#16509,#16510);
#14481=AXIS2_PLACEMENT_3D('',#26083,#16511,#16512);
#14482=AXIS2_PLACEMENT_3D('',#26089,#16516,#16517);
#14483=AXIS2_PLACEMENT_3D('',#26093,#16519,#16520);
#14484=AXIS2_PLACEMENT_3D('',#26094,#16521,#16522);
#14485=AXIS2_PLACEMENT_3D('',#26095,#16523,#16524);
#14486=AXIS2_PLACEMENT_3D('',#26098,#16527,#16528);
#14487=AXIS2_PLACEMENT_3D('',#26115,#16538,#16539);
#14488=AXIS2_PLACEMENT_3D('',#26118,#16541,#16542);
#14489=AXIS2_PLACEMENT_3D('',#26119,#16543,#16544);
#14490=AXIS2_PLACEMENT_3D('',#26123,#16547,#16548);
#14491=AXIS2_PLACEMENT_3D('',#26126,#16550,#16551);
#14492=AXIS2_PLACEMENT_3D('',#26127,#16552,#16553);
#14493=AXIS2_PLACEMENT_3D('',#26142,#16562,#16563);
#14494=AXIS2_PLACEMENT_3D('',#26146,#16566,#16567);
#14495=AXIS2_PLACEMENT_3D('',#26150,#16569,#16570);
#14496=AXIS2_PLACEMENT_3D('',#26151,#16571,#16572);
#14497=AXIS2_PLACEMENT_3D('',#26152,#16573,#16574);
#14498=AXIS2_PLACEMENT_3D('',#26158,#16578,#16579);
#14499=AXIS2_PLACEMENT_3D('',#26161,#16581,#16582);
#14500=AXIS2_PLACEMENT_3D('',#26162,#16583,#16584);
#14501=AXIS2_PLACEMENT_3D('',#26163,#16585,#16586);
#14502=AXIS2_PLACEMENT_3D('',#26165,#16588,#16589);
#14503=AXIS2_PLACEMENT_3D('',#26168,#16591,#16592);
#14504=AXIS2_PLACEMENT_3D('',#26169,#16593,#16594);
#14505=AXIS2_PLACEMENT_3D('',#26173,#16597,#16598);
#14506=AXIS2_PLACEMENT_3D('',#26174,#16599,#16600);
#14507=AXIS2_PLACEMENT_3D('',#26175,#16601,#16602);
#14508=AXIS2_PLACEMENT_3D('',#26179,#16605,#16606);
#14509=AXIS2_PLACEMENT_3D('',#26180,#16607,#16608);
#14510=AXIS2_PLACEMENT_3D('',#26182,#16610,#16611);
#14511=AXIS2_PLACEMENT_3D('',#26184,#16613,#16614);
#14512=AXIS2_PLACEMENT_3D('',#26186,#16616,#16617);
#14513=AXIS2_PLACEMENT_3D('',#26188,#16619,#16620);
#14514=AXIS2_PLACEMENT_3D('',#26190,#16622,#16623);
#14515=AXIS2_PLACEMENT_3D('',#26193,#16625,#16626);
#14516=AXIS2_PLACEMENT_3D('',#26194,#16627,#16628);
#14517=AXIS2_PLACEMENT_3D('',#26196,#16630,#16631);
#14518=AXIS2_PLACEMENT_3D('',#26199,#16633,#16634);
#14519=AXIS2_PLACEMENT_3D('',#26200,#16635,#16636);
#14520=AXIS2_PLACEMENT_3D('',#26206,#16640,#16641);
#14521=AXIS2_PLACEMENT_3D('',#26212,#16645,#16646);
#14522=AXIS2_PLACEMENT_3D('',#26215,#16649,#16650);
#14523=AXIS2_PLACEMENT_3D('',#26219,#16652,#16653);
#14524=AXIS2_PLACEMENT_3D('',#26221,#16655,#16656);
#14525=AXIS2_PLACEMENT_3D('',#26225,#16659,#16660);
#14526=AXIS2_PLACEMENT_3D('',#26228,#16662,#16663);
#14527=AXIS2_PLACEMENT_3D('',#26229,#16664,#16665);
#14528=AXIS2_PLACEMENT_3D('',#26234,#16669,#16670);
#14529=AXIS2_PLACEMENT_3D('',#26237,#16672,#16673);
#14530=AXIS2_PLACEMENT_3D('',#26238,#16674,#16675);
#14531=AXIS2_PLACEMENT_3D('',#26242,#16678,#16679);
#14532=AXIS2_PLACEMENT_3D('',#26245,#16681,#16682);
#14533=AXIS2_PLACEMENT_3D('',#26246,#16683,#16684);
#14534=AXIS2_PLACEMENT_3D('',#26249,#16687,#16688);
#14535=AXIS2_PLACEMENT_3D('',#26251,#16690,#16691);
#14536=AXIS2_PLACEMENT_3D('',#26284,#16708,#16709);
#14537=AXIS2_PLACEMENT_3D('',#26288,#16712,#16713);
#14538=AXIS2_PLACEMENT_3D('',#26292,#16715,#16716);
#14539=AXIS2_PLACEMENT_3D('',#26293,#16717,#16718);
#14540=AXIS2_PLACEMENT_3D('',#26294,#16719,#16720);
#14541=AXIS2_PLACEMENT_3D('',#26299,#16724,#16725);
#14542=AXIS2_PLACEMENT_3D('',#26302,#16727,#16728);
#14543=AXIS2_PLACEMENT_3D('',#26303,#16729,#16730);
#14544=AXIS2_PLACEMENT_3D('',#26305,#16732,#16733);
#14545=AXIS2_PLACEMENT_3D('',#26306,#16734,#16735);
#14546=AXIS2_PLACEMENT_3D('',#26310,#16738,#16739);
#14547=AXIS2_PLACEMENT_3D('',#26313,#16741,#16742);
#14548=AXIS2_PLACEMENT_3D('',#26314,#16743,#16744);
#14549=AXIS2_PLACEMENT_3D('',#26318,#16747,#16748);
#14550=AXIS2_PLACEMENT_3D('',#26321,#16750,#16751);
#14551=AXIS2_PLACEMENT_3D('',#26322,#16752,#16753);
#14552=AXIS2_PLACEMENT_3D('',#26324,#16755,#16756);
#14553=AXIS2_PLACEMENT_3D('',#26325,#16757,#16758);
#14554=AXIS2_PLACEMENT_3D('',#26331,#16762,#16763);
#14555=AXIS2_PLACEMENT_3D('',#26337,#16767,#16768);
#14556=AXIS2_PLACEMENT_3D('',#26339,#16770,#16771);
#14557=AXIS2_PLACEMENT_3D('',#26341,#16773,#16774);
#14558=AXIS2_PLACEMENT_3D('',#26347,#16778,#16779);
#14559=AXIS2_PLACEMENT_3D('',#26352,#16782,#16783);
#14560=AXIS2_PLACEMENT_3D('',#26353,#16784,#16785);
#14561=AXIS2_PLACEMENT_3D('',#26359,#16789,#16790);
#14562=AXIS2_PLACEMENT_3D('',#26365,#16794,#16795);
#14563=AXIS2_PLACEMENT_3D('',#26367,#16797,#16798);
#14564=AXIS2_PLACEMENT_3D('',#26369,#16800,#16801);
#14565=AXIS2_PLACEMENT_3D('',#26375,#16805,#16806);
#14566=AXIS2_PLACEMENT_3D('',#26380,#16809,#16810);
#14567=AXIS2_PLACEMENT_3D('',#26381,#16811,#16812);
#14568=AXIS2_PLACEMENT_3D('',#26387,#16816,#16817);
#14569=AXIS2_PLACEMENT_3D('',#26393,#16821,#16822);
#14570=AXIS2_PLACEMENT_3D('',#26395,#16824,#16825);
#14571=AXIS2_PLACEMENT_3D('',#26397,#16827,#16828);
#14572=AXIS2_PLACEMENT_3D('',#26403,#16832,#16833);
#14573=AXIS2_PLACEMENT_3D('',#26408,#16836,#16837);
#14574=AXIS2_PLACEMENT_3D('',#26409,#16838,#16839);
#14575=AXIS2_PLACEMENT_3D('',#26415,#16843,#16844);
#14576=AXIS2_PLACEMENT_3D('',#26421,#16848,#16849);
#14577=AXIS2_PLACEMENT_3D('',#26423,#16851,#16852);
#14578=AXIS2_PLACEMENT_3D('',#26425,#16854,#16855);
#14579=AXIS2_PLACEMENT_3D('',#26431,#16859,#16860);
#14580=AXIS2_PLACEMENT_3D('',#26436,#16863,#16864);
#14581=AXIS2_PLACEMENT_3D('',#26437,#16865,#16866);
#14582=AXIS2_PLACEMENT_3D('',#26440,#16868,#16869);
#14583=AXIS2_PLACEMENT_3D('',#26441,#16870,#16871);
#14584=AXIS2_PLACEMENT_3D('',#26444,#16873,#16874);
#14585=AXIS2_PLACEMENT_3D('',#26445,#16875,#16876);
#14586=AXIS2_PLACEMENT_3D('',#26448,#16878,#16879);
#14587=AXIS2_PLACEMENT_3D('',#26449,#16880,#16881);
#14588=AXIS2_PLACEMENT_3D('',#26452,#16883,#16884);
#14589=AXIS2_PLACEMENT_3D('',#26453,#16885,#16886);
#14590=AXIS2_PLACEMENT_3D('',#26455,#16888,#16889);
#14591=AXIS2_PLACEMENT_3D('',#26459,#16892,#16893);
#14592=AXIS2_PLACEMENT_3D('',#26461,#16895,#16896);
#14593=AXIS2_PLACEMENT_3D('',#26462,#16897,#16898);
#14594=AXIS2_PLACEMENT_3D('',#26466,#16901,#16902);
#14595=AXIS2_PLACEMENT_3D('',#26468,#16904,#16905);
#14596=AXIS2_PLACEMENT_3D('',#26469,#16906,#16907);
#14597=AXIS2_PLACEMENT_3D('',#26473,#16910,#16911);
#14598=AXIS2_PLACEMENT_3D('',#26475,#16913,#16914);
#14599=AXIS2_PLACEMENT_3D('',#26476,#16915,#16916);
#14600=AXIS2_PLACEMENT_3D('',#26480,#16919,#16920);
#14601=AXIS2_PLACEMENT_3D('',#26482,#16922,#16923);
#14602=AXIS2_PLACEMENT_3D('',#26483,#16924,#16925);
#14603=AXIS2_PLACEMENT_3D('',#26485,#16927,#16928);
#14604=AXIS2_PLACEMENT_3D('',#26486,#16929,#16930);
#14605=AXIS2_PLACEMENT_3D('',#26487,#16931,#16932);
#14606=AXIS2_PLACEMENT_3D('',#26488,#16933,#16934);
#14607=AXIS2_PLACEMENT_3D('',#26489,#16935,#16936);
#14608=AXIS2_PLACEMENT_3D('',#26491,#16938,#16939);
#14609=AXIS2_PLACEMENT_3D('',#26492,#16940,#16941);
#14610=AXIS2_PLACEMENT_3D('',#26493,#16942,#16943);
#14611=AXIS2_PLACEMENT_3D('',#26494,#16944,#16945);
#14612=AXIS2_PLACEMENT_3D('',#26496,#16946,#16947);
#14613=AXIS2_PLACEMENT_3D('',#26500,#16949,#16950);
#14614=AXIS2_PLACEMENT_3D('',#26501,#16951,#16952);
#14615=AXIS2_PLACEMENT_3D('',#26502,#16953,#16954);
#14616=AXIS2_PLACEMENT_3D('',#26506,#16956,#16957);
#14617=AXIS2_PLACEMENT_3D('',#26507,#16958,#16959);
#14618=AXIS2_PLACEMENT_3D('',#26508,#16960,#16961);
#14619=AXIS2_PLACEMENT_3D('',#26509,#16962,#16963);
#14620=AXIS2_PLACEMENT_3D('',#26513,#16965,#16966);
#14621=AXIS2_PLACEMENT_3D('',#26514,#16967,#16968);
#14622=AXIS2_PLACEMENT_3D('',#26515,#16969,#16970);
#14623=AXIS2_PLACEMENT_3D('',#26518,#16972,#16973);
#14624=AXIS2_PLACEMENT_3D('',#26519,#16974,#16975);
#14625=AXIS2_PLACEMENT_3D('',#26521,#16976,#16977);
#14626=AXIS2_PLACEMENT_3D('',#26522,#16978,#16979);
#14627=AXIS2_PLACEMENT_3D('',#26524,#16981,#16982);
#14628=AXIS2_PLACEMENT_3D('',#26525,#16983,#16984);
#14629=AXIS2_PLACEMENT_3D('',#26527,#16985,#16986);
#14630=AXIS2_PLACEMENT_3D('',#26528,#16987,#16988);
#14631=AXIS2_PLACEMENT_3D('',#26530,#16989,#16990);
#14632=AXIS2_PLACEMENT_3D('',#26532,#16992,#16993);
#14633=AXIS2_PLACEMENT_3D('',#26534,#16994,#16995);
#14634=AXIS2_PLACEMENT_3D('',#26536,#16997,#16998);
#14635=AXIS2_PLACEMENT_3D('',#26538,#16999,#17000);
#14636=AXIS2_PLACEMENT_3D('',#26540,#17002,#17003);
#14637=AXIS2_PLACEMENT_3D('',#26541,#17004,#17005);
#14638=AXIS2_PLACEMENT_3D('',#26542,#17006,#17007);
#14639=AXIS2_PLACEMENT_3D('',#26551,#17012,#17013);
#14640=AXIS2_PLACEMENT_3D('',#26557,#17017,#17018);
#14641=AXIS2_PLACEMENT_3D('',#26563,#17022,#17023);
#14642=AXIS2_PLACEMENT_3D('',#26569,#17027,#17028);
#14643=AXIS2_PLACEMENT_3D('',#26575,#17032,#17033);
#14644=AXIS2_PLACEMENT_3D('',#26581,#17037,#17038);
#14645=AXIS2_PLACEMENT_3D('',#26587,#17042,#17043);
#14646=AXIS2_PLACEMENT_3D('',#26593,#17047,#17048);
#14647=AXIS2_PLACEMENT_3D('',#26599,#17052,#17053);
#14648=AXIS2_PLACEMENT_3D('',#26605,#17057,#17058);
#14649=AXIS2_PLACEMENT_3D('',#26611,#17062,#17063);
#14650=AXIS2_PLACEMENT_3D('',#26617,#17067,#17068);
#14651=AXIS2_PLACEMENT_3D('',#26623,#17072,#17073);
#14652=AXIS2_PLACEMENT_3D('',#26629,#17077,#17078);
#14653=AXIS2_PLACEMENT_3D('',#26635,#17082,#17083);
#14654=AXIS2_PLACEMENT_3D('',#26641,#17087,#17088);
#14655=AXIS2_PLACEMENT_3D('',#26647,#17092,#17093);
#14656=AXIS2_PLACEMENT_3D('',#26653,#17097,#17098);
#14657=AXIS2_PLACEMENT_3D('',#26659,#17102,#17103);
#14658=AXIS2_PLACEMENT_3D('',#26665,#17107,#17108);
#14659=AXIS2_PLACEMENT_3D('',#26671,#17112,#17113);
#14660=AXIS2_PLACEMENT_3D('',#26677,#17117,#17118);
#14661=AXIS2_PLACEMENT_3D('',#26683,#17122,#17123);
#14662=AXIS2_PLACEMENT_3D('',#26689,#17127,#17128);
#14663=AXIS2_PLACEMENT_3D('',#26695,#17132,#17133);
#14664=AXIS2_PLACEMENT_3D('',#26701,#17137,#17138);
#14665=AXIS2_PLACEMENT_3D('',#26707,#17142,#17143);
#14666=AXIS2_PLACEMENT_3D('',#26713,#17147,#17148);
#14667=AXIS2_PLACEMENT_3D('',#26719,#17152,#17153);
#14668=AXIS2_PLACEMENT_3D('',#26725,#17157,#17158);
#14669=AXIS2_PLACEMENT_3D('',#26731,#17162,#17163);
#14670=AXIS2_PLACEMENT_3D('',#26737,#17167,#17168);
#14671=AXIS2_PLACEMENT_3D('',#26743,#17172,#17173);
#14672=AXIS2_PLACEMENT_3D('',#26749,#17177,#17178);
#14673=AXIS2_PLACEMENT_3D('',#26755,#17182,#17183);
#14674=AXIS2_PLACEMENT_3D('',#26761,#17187,#17188);
#14675=AXIS2_PLACEMENT_3D('',#26767,#17192,#17193);
#14676=AXIS2_PLACEMENT_3D('',#26773,#17197,#17198);
#14677=AXIS2_PLACEMENT_3D('',#26779,#17202,#17203);
#14678=AXIS2_PLACEMENT_3D('',#26785,#17207,#17208);
#14679=AXIS2_PLACEMENT_3D('',#26791,#17212,#17213);
#14680=AXIS2_PLACEMENT_3D('',#26797,#17217,#17218);
#14681=AXIS2_PLACEMENT_3D('',#26803,#17222,#17223);
#14682=AXIS2_PLACEMENT_3D('',#26809,#17227,#17228);
#14683=AXIS2_PLACEMENT_3D('',#26815,#17232,#17233);
#14684=AXIS2_PLACEMENT_3D('',#26821,#17237,#17238);
#14685=AXIS2_PLACEMENT_3D('',#26827,#17242,#17243);
#14686=AXIS2_PLACEMENT_3D('',#26833,#17247,#17248);
#14687=AXIS2_PLACEMENT_3D('',#26839,#17252,#17253);
#14688=AXIS2_PLACEMENT_3D('',#26842,#17256,#17257);
#14689=AXIS2_PLACEMENT_3D('',#26843,#17258,#17259);
#14690=AXIS2_PLACEMENT_3D('',#26844,#17260,#17261);
#14691=AXIS2_PLACEMENT_3D('',#26845,#17262,#17263);
#14692=AXIS2_PLACEMENT_3D('',#26854,#17268,#17269);
#14693=AXIS2_PLACEMENT_3D('',#26858,#17271,#17272);
#14694=AXIS2_PLACEMENT_3D('',#26859,#17273,#17274);
#14695=AXIS2_PLACEMENT_3D('',#26860,#17275,#17276);
#14696=AXIS2_PLACEMENT_3D('',#26866,#17280,#17281);
#14697=AXIS2_PLACEMENT_3D('',#26870,#17283,#17284);
#14698=AXIS2_PLACEMENT_3D('',#26871,#17285,#17286);
#14699=AXIS2_PLACEMENT_3D('',#26872,#17287,#17288);
#14700=AXIS2_PLACEMENT_3D('',#26878,#17292,#17293);
#14701=AXIS2_PLACEMENT_3D('',#26882,#17295,#17296);
#14702=AXIS2_PLACEMENT_3D('',#26883,#17297,#17298);
#14703=AXIS2_PLACEMENT_3D('',#26884,#17299,#17300);
#14704=AXIS2_PLACEMENT_3D('',#26890,#17304,#17305);
#14705=AXIS2_PLACEMENT_3D('',#26891,#17306,#17307);
#14706=AXIS2_PLACEMENT_3D('',#26892,#17308,#17309);
#14707=AXIS2_PLACEMENT_3D('',#26893,#17310,#17311);
#14708=AXIS2_PLACEMENT_3D('',#26897,#17313,#17314);
#14709=AXIS2_PLACEMENT_3D('',#26899,#17316,#17317);
#14710=AXIS2_PLACEMENT_3D('',#26903,#17320,#17321);
#14711=AXIS2_PLACEMENT_3D('',#26906,#17323,#17324);
#14712=AXIS2_PLACEMENT_3D('',#26907,#17325,#17326);
#14713=AXIS2_PLACEMENT_3D('',#26911,#17329,#17330);
#14714=AXIS2_PLACEMENT_3D('',#26916,#17332,#17333);
#14715=AXIS2_PLACEMENT_3D('',#26920,#17335,#17336);
#14716=AXIS2_PLACEMENT_3D('',#26924,#17338,#17339);
#14717=AXIS2_PLACEMENT_3D('',#26927,#17341,#17342);
#14718=AXIS2_PLACEMENT_3D('',#26928,#17343,#17344);
#14719=AXIS2_PLACEMENT_3D('',#26933,#17346,#17347);
#14720=AXIS2_PLACEMENT_3D('',#26936,#17349,#17350);
#14721=AXIS2_PLACEMENT_3D('',#26937,#17351,#17352);
#14722=AXIS2_PLACEMENT_3D('',#26943,#17356,#17357);
#14723=AXIS2_PLACEMENT_3D('',#26947,#17359,#17360);
#14724=AXIS2_PLACEMENT_3D('',#26948,#17361,#17362);
#14725=AXIS2_PLACEMENT_3D('',#26949,#17363,#17364);
#14726=AXIS2_PLACEMENT_3D('',#26955,#17368,#17369);
#14727=AXIS2_PLACEMENT_3D('',#26959,#17371,#17372);
#14728=AXIS2_PLACEMENT_3D('',#26960,#17373,#17374);
#14729=AXIS2_PLACEMENT_3D('',#26961,#17375,#17376);
#14730=AXIS2_PLACEMENT_3D('',#26967,#17380,#17381);
#14731=AXIS2_PLACEMENT_3D('',#26971,#17383,#17384);
#14732=AXIS2_PLACEMENT_3D('',#26972,#17385,#17386);
#14733=AXIS2_PLACEMENT_3D('',#26973,#17387,#17388);
#14734=AXIS2_PLACEMENT_3D('',#26976,#17391,#17392);
#14735=AXIS2_PLACEMENT_3D('',#26979,#17395,#17396);
#14736=AXIS2_PLACEMENT_3D('',#26981,#17398,#17399);
#14737=AXIS2_PLACEMENT_3D('',#26983,#17401,#17402);
#14738=AXIS2_PLACEMENT_3D('',#26985,#17404,#17405);
#14739=AXIS2_PLACEMENT_3D('',#26988,#17406,#17407);
#14740=AXIS2_PLACEMENT_3D('',#26992,#17409,#17410);
#14741=AXIS2_PLACEMENT_3D('',#26996,#17412,#17413);
#14742=AXIS2_PLACEMENT_3D('',#27000,#17415,#17416);
#14743=AXIS2_PLACEMENT_3D('',#27002,#17418,#17419);
#14744=AXIS2_PLACEMENT_3D('',#27007,#17422,#17423);
#14745=AXIS2_PLACEMENT_3D('',#27008,#17424,#17425);
#14746=AXIS2_PLACEMENT_3D('',#27012,#17428,#17429);
#14747=AXIS2_PLACEMENT_3D('',#27015,#17431,#17432);
#14748=AXIS2_PLACEMENT_3D('',#27016,#17433,#17434);
#14749=AXIS2_PLACEMENT_3D('',#27020,#17437,#17438);
#14750=AXIS2_PLACEMENT_3D('',#27023,#17440,#17441);
#14751=AXIS2_PLACEMENT_3D('',#27024,#17442,#17443);
#14752=AXIS2_PLACEMENT_3D('',#27028,#17446,#17447);
#14753=AXIS2_PLACEMENT_3D('',#27031,#17449,#17450);
#14754=AXIS2_PLACEMENT_3D('',#27032,#17451,#17452);
#14755=AXIS2_PLACEMENT_3D('',#27034,#17454,#17455);
#14756=AXIS2_PLACEMENT_3D('',#27044,#17461,#17462);
#14757=AXIS2_PLACEMENT_3D('',#27127,#17464,#17465);
#14758=AXIS2_PLACEMENT_3D('',#27208,#17466,#17467);
#14759=AXIS2_PLACEMENT_3D('',#27216,#17472,#17473);
#14760=AXIS2_PLACEMENT_3D('',#27300,#17475,#17476);
#14761=AXIS2_PLACEMENT_3D('',#27835,#17479,#17480);
#14762=AXIS2_PLACEMENT_3D('',#27840,#17482,#17483);
#14763=AXIS2_PLACEMENT_3D('',#27843,#17485,#17486);
#14764=AXIS2_PLACEMENT_3D('',#27943,#17488,#17489);
#14765=AXIS2_PLACEMENT_3D('',#28051,#17491,#17492);
#14766=AXIS2_PLACEMENT_3D('',#28530,#17497,#17498);
#14767=AXIS2_PLACEMENT_3D('',#28535,#17500,#17501);
#14768=AXIS2_PLACEMENT_3D('',#28538,#17503,#17504);
#14769=AXIS2_PLACEMENT_3D('',#28620,#17506,#17507);
#14770=AXIS2_PLACEMENT_3D('',#28623,#17510,#17511);
#14771=AXIS2_PLACEMENT_3D('',#28625,#17513,#17514);
#14772=AXIS2_PLACEMENT_3D('',#28627,#17516,#17517);
#14773=AXIS2_PLACEMENT_3D('',#28631,#17519,#17520);
#14774=AXIS2_PLACEMENT_3D('',#28633,#17522,#17523);
#14775=AXIS2_PLACEMENT_3D('',#28637,#17526,#17527);
#14776=AXIS2_PLACEMENT_3D('',#28640,#17529,#17530);
#14777=AXIS2_PLACEMENT_3D('',#28641,#17531,#17532);
#14778=AXIS2_PLACEMENT_3D('',#28645,#17535,#17536);
#14779=AXIS2_PLACEMENT_3D('',#28649,#17538,#17539);
#14780=AXIS2_PLACEMENT_3D('',#28650,#17540,#17541);
#14781=AXIS2_PLACEMENT_3D('',#28651,#17542,#17543);
#14782=AXIS2_PLACEMENT_3D('',#28657,#17547,#17548);
#14783=AXIS2_PLACEMENT_3D('',#28661,#17550,#17551);
#14784=AXIS2_PLACEMENT_3D('',#28662,#17552,#17553);
#14785=AXIS2_PLACEMENT_3D('',#28663,#17554,#17555);
#14786=AXIS2_PLACEMENT_3D('',#28666,#17558,#17559);
#14787=AXIS2_PLACEMENT_3D('',#28673,#17560,#17561);
#14788=AXIS2_PLACEMENT_3D('',#28687,#17563,#17564);
#14789=AXIS2_PLACEMENT_3D('',#28909,#17567,#17568);
#14790=AXIS2_PLACEMENT_3D('',#28970,#17572,#17573);
#14791=AXIS2_PLACEMENT_3D('',#29283,#17576,#17577);
#14792=AXIS2_PLACEMENT_3D('',#29349,#17581,#17582);
#14793=AXIS2_PLACEMENT_3D('',#29351,#17584,#17585);
#14794=AXIS2_PLACEMENT_3D('',#29352,#17586,#17587);
#14795=AXIS2_PLACEMENT_3D('',#29354,#17589,#17590);
#14796=AXIS2_PLACEMENT_3D('',#29356,#17592,#17593);
#14797=AXIS2_PLACEMENT_3D('',#29358,#17595,#17596);
#14798=AXIS2_PLACEMENT_3D('',#29359,#17597,#17598);
#14799=AXIS2_PLACEMENT_3D('',#29362,#17601,#17602);
#14800=AXIS2_PLACEMENT_3D('',#29364,#17604,#17605);
#14801=AXIS2_PLACEMENT_3D('',#29365,#17606,#17607);
#14802=AXIS2_PLACEMENT_3D('',#29366,#17608,#17609);
#14803=AXIS2_PLACEMENT_3D('',#29367,#17610,#17611);
#14804=AXIS2_PLACEMENT_3D('',#29380,#17618,#17619);
#14805=AXIS2_PLACEMENT_3D('',#29384,#17621,#17622);
#14806=AXIS2_PLACEMENT_3D('',#29385,#17623,#17624);
#14807=AXIS2_PLACEMENT_3D('',#29386,#17625,#17626);
#14808=AXIS2_PLACEMENT_3D('',#29392,#17630,#17631);
#14809=AXIS2_PLACEMENT_3D('',#29396,#17633,#17634);
#14810=AXIS2_PLACEMENT_3D('',#29397,#17635,#17636);
#14811=AXIS2_PLACEMENT_3D('',#29398,#17637,#17638);
#14812=AXIS2_PLACEMENT_3D('',#29404,#17642,#17643);
#14813=AXIS2_PLACEMENT_3D('',#29408,#17645,#17646);
#14814=AXIS2_PLACEMENT_3D('',#29409,#17647,#17648);
#14815=AXIS2_PLACEMENT_3D('',#29410,#17649,#17650);
#14816=AXIS2_PLACEMENT_3D('',#29416,#17654,#17655);
#14817=AXIS2_PLACEMENT_3D('',#29417,#17656,#17657);
#14818=AXIS2_PLACEMENT_3D('',#29418,#17658,#17659);
#14819=AXIS2_PLACEMENT_3D('',#29419,#17660,#17661);
#14820=AXIS2_PLACEMENT_3D('',#29427,#17665,#17666);
#14821=AXIS2_PLACEMENT_3D('',#29431,#17668,#17669);
#14822=AXIS2_PLACEMENT_3D('',#29435,#17671,#17672);
#14823=AXIS2_PLACEMENT_3D('',#29439,#17674,#17675);
#14824=AXIS2_PLACEMENT_3D('',#29445,#17679,#17680);
#14825=AXIS2_PLACEMENT_3D('',#29449,#17682,#17683);
#14826=AXIS2_PLACEMENT_3D('',#29451,#17685,#17686);
#14827=AXIS2_PLACEMENT_3D('',#29455,#17689,#17690);
#14828=AXIS2_PLACEMENT_3D('',#29458,#17692,#17693);
#14829=AXIS2_PLACEMENT_3D('',#29459,#17694,#17695);
#14830=AXIS2_PLACEMENT_3D('',#29463,#17698,#17699);
#14831=AXIS2_PLACEMENT_3D('',#29470,#17703,#17704);
#14832=AXIS2_PLACEMENT_3D('',#29478,#17709,#17710);
#14833=AXIS2_PLACEMENT_3D('',#29486,#17715,#17716);
#14834=AXIS2_PLACEMENT_3D('',#29489,#17719,#17720);
#14835=AXIS2_PLACEMENT_3D('',#29493,#17723,#17724);
#14836=AXIS2_PLACEMENT_3D('',#29499,#17728,#17729);
#14837=AXIS2_PLACEMENT_3D('',#29502,#17732,#17733);
#14838=AXIS2_PLACEMENT_3D('',#29946,#17737,#17738);
#14839=AXIS2_PLACEMENT_3D('',#29951,#17740,#17741);
#14840=AXIS2_PLACEMENT_3D('',#29954,#17743,#17744);
#14841=AXIS2_PLACEMENT_3D('',#30036,#17746,#17747);
#14842=AXIS2_PLACEMENT_3D('',#30141,#17750,#17751);
#14843=AXIS2_PLACEMENT_3D('',#30149,#17756,#17757);
#14844=AXIS2_PLACEMENT_3D('',#30152,#17759,#17760);
#14845=AXIS2_PLACEMENT_3D('',#30500,#17763,#17764);
#14846=AXIS2_PLACEMENT_3D('',#30505,#17766,#17767);
#14847=AXIS2_PLACEMENT_3D('',#30508,#17769,#17770);
#14848=AXIS2_PLACEMENT_3D('',#30590,#17772,#17773);
#14849=AXIS2_PLACEMENT_3D('',#30599,#17775,#17776);
#14850=AXIS2_PLACEMENT_3D('',#30613,#17778,#17779);
#14851=AXIS2_PLACEMENT_3D('',#30620,#17781,#17782);
#14852=AXIS2_PLACEMENT_3D('',#30624,#17785,#17786);
#14853=AXIS2_PLACEMENT_3D('',#30628,#17789,#17790);
#14854=AXIS2_PLACEMENT_3D('',#30634,#17794,#17795);
#14855=AXIS2_PLACEMENT_3D('',#30637,#17797,#17798);
#14856=AXIS2_PLACEMENT_3D('',#30638,#17799,#17800);
#14857=AXIS2_PLACEMENT_3D('',#30642,#17803,#17804);
#14858=AXIS2_PLACEMENT_3D('',#30644,#17806,#17807);
#14859=AXIS2_PLACEMENT_3D('',#30645,#17808,#17809);
#14860=AXIS2_PLACEMENT_3D('',#30647,#17811,#17812);
#14861=AXIS2_PLACEMENT_3D('',#30649,#17814,#17815);
#14862=AXIS2_PLACEMENT_3D('',#30653,#17818,#17819);
#14863=AXIS2_PLACEMENT_3D('',#30656,#17821,#17822);
#14864=AXIS2_PLACEMENT_3D('',#30657,#17823,#17824);
#14865=AXIS2_PLACEMENT_3D('',#30661,#17827,#17828);
#14866=AXIS2_PLACEMENT_3D('',#30664,#17831,#17832);
#14867=AXIS2_PLACEMENT_3D('',#30667,#17835,#17836);
#14868=AXIS2_PLACEMENT_3D('',#30669,#17838,#17839);
#14869=AXIS2_PLACEMENT_3D('',#30675,#17843,#17844);
#14870=AXIS2_PLACEMENT_3D('',#30761,#17846,#17847);
#14871=AXIS2_PLACEMENT_3D('',#30850,#17848,#17849);
#14872=AXIS2_PLACEMENT_3D('',#30851,#17850,#17851);
#14873=AXIS2_PLACEMENT_3D('',#31302,#17855,#17856);
#14874=AXIS2_PLACEMENT_3D('',#31306,#17858,#17859);
#14875=AXIS2_PLACEMENT_3D('',#31380,#17862,#17863);
#14876=AXIS2_PLACEMENT_3D('',#31382,#17865,#17866);
#14877=AXIS2_PLACEMENT_3D('',#31384,#17868,#17869);
#14878=AXIS2_PLACEMENT_3D('',#31684,#17873,#17874);
#14879=AXIS2_PLACEMENT_3D('',#31745,#17878,#17879);
#14880=AXIS2_PLACEMENT_3D('',#31746,#17880,#17881);
#14881=AXIS2_PLACEMENT_3D('',#31748,#17883,#17884);
#14882=AXIS2_PLACEMENT_3D('',#31749,#17885,#17886);
#14883=AXIS2_PLACEMENT_3D('',#31752,#17888,#17889);
#14884=AXIS2_PLACEMENT_3D('',#31753,#17890,#17891);
#14885=AXIS2_PLACEMENT_3D('',#31757,#17894,#17895);
#14886=AXIS2_PLACEMENT_3D('',#31760,#17897,#17898);
#14887=AXIS2_PLACEMENT_3D('',#31761,#17899,#17900);
#14888=AXIS2_PLACEMENT_3D('',#31763,#17902,#17903);
#14889=AXIS2_PLACEMENT_3D('',#31764,#17904,#17905);
#14890=AXIS2_PLACEMENT_3D('',#31765,#17906,#17907);
#14891=AXIS2_PLACEMENT_3D('',#31767,#17908,#17909);
#14892=AXIS2_PLACEMENT_3D('',#31770,#17911,#17912);
#14893=AXIS2_PLACEMENT_3D('',#31771,#17913,#17914);
#14894=AXIS2_PLACEMENT_3D('',#31773,#17915,#17916);
#14895=AXIS2_PLACEMENT_3D('',#31775,#17918,#17919);
#14896=AXIS2_PLACEMENT_3D('',#31796,#17930,#17931);
#14897=AXIS2_PLACEMENT_3D('',#31798,#17932,#17933);
#14898=AXIS2_PLACEMENT_3D('',#31800,#17935,#17936);
#14899=AXIS2_PLACEMENT_3D('',#31921,#17997,#17998);
#14900=AXIS2_PLACEMENT_3D('',#31927,#18002,#18003);
#14901=AXIS2_PLACEMENT_3D('',#31933,#18007,#18008);
#14902=AXIS2_PLACEMENT_3D('',#31939,#18012,#18013);
#14903=AXIS2_PLACEMENT_3D('',#31945,#18017,#18018);
#14904=AXIS2_PLACEMENT_3D('',#31951,#18022,#18023);
#14905=AXIS2_PLACEMENT_3D('',#31957,#18027,#18028);
#14906=AXIS2_PLACEMENT_3D('',#31963,#18032,#18033);
#14907=AXIS2_PLACEMENT_3D('',#31969,#18037,#18038);
#14908=AXIS2_PLACEMENT_3D('',#31975,#18042,#18043);
#14909=AXIS2_PLACEMENT_3D('',#31977,#18045,#18046);
#14910=AXIS2_PLACEMENT_3D('',#31983,#18050,#18051);
#14911=AXIS2_PLACEMENT_3D('',#31985,#18053,#18054);
#14912=AXIS2_PLACEMENT_3D('',#31991,#18058,#18059);
#14913=AXIS2_PLACEMENT_3D('',#31994,#18062,#18063);
#14914=AXIS2_PLACEMENT_3D('',#31997,#18066,#18067);
#14915=AXIS2_PLACEMENT_3D('',#32000,#18070,#18071);
#14916=AXIS2_PLACEMENT_3D('',#32006,#18075,#18076);
#14917=AXIS2_PLACEMENT_3D('',#32012,#18080,#18081);
#14918=AXIS2_PLACEMENT_3D('',#32019,#18086,#18087);
#14919=AXIS2_PLACEMENT_3D('',#32023,#18090,#18091);
#14920=AXIS2_PLACEMENT_3D('',#32027,#18094,#18095);
#14921=AXIS2_PLACEMENT_3D('',#32033,#18099,#18100);
#14922=AXIS2_PLACEMENT_3D('',#32039,#18104,#18105);
#14923=AXIS2_PLACEMENT_3D('',#32045,#18109,#18110);
#14924=AXIS2_PLACEMENT_3D('',#32051,#18114,#18115);
#14925=AXIS2_PLACEMENT_3D('',#32057,#18119,#18120);
#14926=AXIS2_PLACEMENT_3D('',#32063,#18124,#18125);
#14927=AXIS2_PLACEMENT_3D('',#32069,#18129,#18130);
#14928=AXIS2_PLACEMENT_3D('',#32075,#18134,#18135);
#14929=AXIS2_PLACEMENT_3D('',#32081,#18139,#18140);
#14930=AXIS2_PLACEMENT_3D('',#32087,#18144,#18145);
#14931=AXIS2_PLACEMENT_3D('',#32093,#18149,#18150);
#14932=AXIS2_PLACEMENT_3D('',#32099,#18154,#18155);
#14933=AXIS2_PLACEMENT_3D('',#32103,#18158,#18159);
#14934=AXIS2_PLACEMENT_3D('',#32109,#18163,#18164);
#14935=AXIS2_PLACEMENT_3D('',#32111,#18166,#18167);
#14936=AXIS2_PLACEMENT_3D('',#32117,#18171,#18172);
#14937=AXIS2_PLACEMENT_3D('',#32119,#18174,#18175);
#14938=AXIS2_PLACEMENT_3D('',#32125,#18179,#18180);
#14939=AXIS2_PLACEMENT_3D('',#32127,#18182,#18183);
#14940=AXIS2_PLACEMENT_3D('',#32133,#18187,#18188);
#14941=AXIS2_PLACEMENT_3D('',#32137,#18191,#18192);
#14942=AXIS2_PLACEMENT_3D('',#32140,#18195,#18196);
#14943=AXIS2_PLACEMENT_3D('',#32142,#18198,#18199);
#14944=AXIS2_PLACEMENT_3D('',#32145,#18202,#18203);
#14945=AXIS2_PLACEMENT_3D('',#32148,#18206,#18207);
#14946=AXIS2_PLACEMENT_3D('',#32151,#18210,#18211);
#14947=AXIS2_PLACEMENT_3D('',#32154,#18214,#18215);
#14948=AXIS2_PLACEMENT_3D('',#32157,#18218,#18219);
#14949=AXIS2_PLACEMENT_3D('',#32163,#18223,#18224);
#14950=AXIS2_PLACEMENT_3D('',#32169,#18228,#18229);
#14951=AXIS2_PLACEMENT_3D('',#32175,#18233,#18234);
#14952=AXIS2_PLACEMENT_3D('',#32181,#18238,#18239);
#14953=AXIS2_PLACEMENT_3D('',#32187,#18243,#18244);
#14954=AXIS2_PLACEMENT_3D('',#32193,#18248,#18249);
#14955=AXIS2_PLACEMENT_3D('',#32199,#18253,#18254);
#14956=AXIS2_PLACEMENT_3D('',#32205,#18258,#18259);
#14957=AXIS2_PLACEMENT_3D('',#32207,#18261,#18262);
#14958=AXIS2_PLACEMENT_3D('',#32209,#18264,#18265);
#14959=AXIS2_PLACEMENT_3D('',#32210,#18266,#18267);
#14960=AXIS2_PLACEMENT_3D('',#32213,#18270,#18271);
#14961=AXIS2_PLACEMENT_3D('',#32214,#18272,#18273);
#14962=AXIS2_PLACEMENT_3D('',#32215,#18274,#18275);
#14963=AXIS2_PLACEMENT_3D('',#32218,#18278,#18279);
#14964=AXIS2_PLACEMENT_3D('',#32219,#18280,#18281);
#14965=AXIS2_PLACEMENT_3D('',#32220,#18282,#18283);
#14966=AXIS2_PLACEMENT_3D('',#32223,#18286,#18287);
#14967=AXIS2_PLACEMENT_3D('',#32224,#18288,#18289);
#14968=AXIS2_PLACEMENT_3D('',#32225,#18290,#18291);
#14969=AXIS2_PLACEMENT_3D('',#32228,#18294,#18295);
#14970=AXIS2_PLACEMENT_3D('',#32229,#18296,#18297);
#14971=AXIS2_PLACEMENT_3D('',#32230,#18298,#18299);
#14972=AXIS2_PLACEMENT_3D('',#32233,#18302,#18303);
#14973=AXIS2_PLACEMENT_3D('',#32234,#18304,#18305);
#14974=AXIS2_PLACEMENT_3D('',#32235,#18306,#18307);
#14975=AXIS2_PLACEMENT_3D('',#32238,#18310,#18311);
#14976=AXIS2_PLACEMENT_3D('',#32239,#18312,#18313);
#14977=AXIS2_PLACEMENT_3D('',#32240,#18314,#18315);
#14978=AXIS2_PLACEMENT_3D('',#32243,#18318,#18319);
#14979=AXIS2_PLACEMENT_3D('',#32244,#18320,#18321);
#14980=AXIS2_PLACEMENT_3D('',#32245,#18322,#18323);
#14981=AXIS2_PLACEMENT_3D('',#32248,#18326,#18327);
#14982=AXIS2_PLACEMENT_3D('',#32249,#18328,#18329);
#14983=AXIS2_PLACEMENT_3D('',#32250,#18330,#18331);
#14984=AXIS2_PLACEMENT_3D('',#32254,#18334,#18335);
#14985=AXIS2_PLACEMENT_3D('',#32258,#18338,#18339);
#14986=AXIS2_PLACEMENT_3D('',#32260,#18341,#18342);
#14987=AXIS2_PLACEMENT_3D('',#32261,#18343,#18344);
#14988=AXIS2_PLACEMENT_3D('',#32262,#18345,#18346);
#14989=AXIS2_PLACEMENT_3D('',#32263,#18347,#18348);
#14990=AXIS2_PLACEMENT_3D('',#32264,#18349,#18350);
#14991=AXIS2_PLACEMENT_3D('',#32265,#18351,#18352);
#14992=AXIS2_PLACEMENT_3D('',#32266,#18353,#18354);
#14993=AXIS2_PLACEMENT_3D('',#32267,#18355,#18356);
#14994=AXIS2_PLACEMENT_3D('',#32268,#18357,#18358);
#14995=AXIS2_PLACEMENT_3D('',#32269,#18359,#18360);
#14996=AXIS2_PLACEMENT_3D('',#32270,#18361,#18362);
#14997=AXIS2_PLACEMENT_3D('',#32271,#18363,#18364);
#14998=AXIS2_PLACEMENT_3D('',#32272,#18365,#18366);
#14999=AXIS2_PLACEMENT_3D('',#32273,#18367,#18368);
#15000=AXIS2_PLACEMENT_3D('',#32274,#18369,#18370);
#15001=AXIS2_PLACEMENT_3D('',#32275,#18371,#18372);
#15002=AXIS2_PLACEMENT_3D('',#32276,#18373,#18374);
#15003=AXIS2_PLACEMENT_3D('',#32277,#18375,#18376);
#15004=DIRECTION('axis',(0.,0.,1.));
#15005=DIRECTION('refdir',(1.,0.,0.));
#15006=DIRECTION('axis',(0.,0.,1.));
#15007=DIRECTION('refdir',(1.,0.,0.));
#15008=DIRECTION('center_axis',(0.707106781186541,-0.707106781186554,0.));
#15009=DIRECTION('ref_axis',(0.,0.,-1.));
#15010=DIRECTION('',(0.707106781186554,0.707106781186541,-6.28036983473507E-15));
#15011=DIRECTION('',(0.,0.,1.));
#15012=DIRECTION('',(-0.707106781186554,-0.707106781186541,0.));
#15013=DIRECTION('',(0.,0.,-1.));
#15014=DIRECTION('center_axis',(1.,0.,0.));
#15015=DIRECTION('ref_axis',(0.,-3.96951249027992E-15,-1.));
#15016=DIRECTION('',(0.707106781186554,0.,-0.707106781186541));
#15017=DIRECTION('center_axis',(1.,0.,0.));
#15018=DIRECTION('ref_axis',(0.,-3.96951249027992E-15,-1.));
#15019=DIRECTION('center_axis',(-1.,0.,0.));
#15020=DIRECTION('ref_axis',(0.,-3.96951249027992E-15,-1.));
#15021=DIRECTION('center_axis',(0.707106781186541,0.,0.707106781186554));
#15022=DIRECTION('ref_axis',(0.707106781186554,0.,-0.707106781186541));
#15023=DIRECTION('',(0.707106781186554,3.14018491736753E-15,-0.707106781186541));
#15024=DIRECTION('',(0.,1.,0.));
#15025=DIRECTION('',(0.,-1.,0.));
#15026=DIRECTION('center_axis',(1.,0.,0.));
#15027=DIRECTION('ref_axis',(0.,-1.,-1.98475624513994E-15));
#15028=DIRECTION('',(0.707106781186553,-0.707106781186542,0.));
#15029=DIRECTION('center_axis',(1.,0.,0.));
#15030=DIRECTION('ref_axis',(0.,-1.,-1.98475624513994E-15));
#15031=DIRECTION('center_axis',(-1.,0.,0.));
#15032=DIRECTION('ref_axis',(0.,-1.,-1.98475624513994E-15));
#15033=DIRECTION('center_axis',(0.707106781186542,0.707106781186553,0.));
#15034=DIRECTION('ref_axis',(0.,0.,-1.));
#15035=DIRECTION('',(0.707106781186554,-0.707106781186541,0.));
#15036=DIRECTION('',(0.,0.,-1.));
#15037=DIRECTION('',(0.,0.,1.));
#15038=DIRECTION('center_axis',(1.,0.,0.));
#15039=DIRECTION('ref_axis',(0.,-9.92378122569971E-16,1.));
#15040=DIRECTION('',(0.707106781186554,0.,0.707106781186541));
#15041=DIRECTION('center_axis',(1.,0.,0.));
#15042=DIRECTION('ref_axis',(0.,-9.92378122569971E-16,1.));
#15043=DIRECTION('center_axis',(-1.,0.,0.));
#15044=DIRECTION('ref_axis',(0.,-9.92378122569971E-16,1.));
#15045=DIRECTION('center_axis',(0.707106781186541,0.,-0.707106781186554));
#15046=DIRECTION('ref_axis',(-0.707106781186554,0.,-0.707106781186541));
#15047=DIRECTION('',(0.707106781186551,0.,0.707106781186544));
#15048=DIRECTION('',(0.,-1.,0.));
#15049=DIRECTION('',(0.,1.,0.));
#15050=DIRECTION('center_axis',(1.,0.,0.));
#15051=DIRECTION('ref_axis',(0.,1.,-5.95426873541988E-15));
#15052=DIRECTION('center_axis',(1.,0.,0.));
#15053=DIRECTION('ref_axis',(0.,1.,-5.95426873541988E-15));
#15054=DIRECTION('center_axis',(-1.,0.,0.));
#15055=DIRECTION('ref_axis',(0.,1.,-5.95426873541988E-15));
#15056=DIRECTION('center_axis',(1.,0.,0.));
#15057=DIRECTION('ref_axis',(0.,-1.,-1.98475624513994E-15));
#15058=DIRECTION('',(1.,0.,0.));
#15059=DIRECTION('center_axis',(1.,0.,0.));
#15060=DIRECTION('ref_axis',(0.,-1.,-1.98475624513994E-15));
#15061=DIRECTION('',(1.,0.,0.));
#15062=DIRECTION('center_axis',(0.,0.,1.));
#15063=DIRECTION('ref_axis',(0.,-1.,0.));
#15064=DIRECTION('',(1.,0.,0.));
#15065=DIRECTION('',(0.,1.,0.));
#15066=DIRECTION('center_axis',(0.,0.,-1.));
#15067=DIRECTION('ref_axis',(1.,0.,0.));
#15068=DIRECTION('center_axis',(1.,0.,0.));
#15069=DIRECTION('ref_axis',(0.,-3.96951249027992E-15,-1.));
#15070=DIRECTION('',(1.,0.,0.));
#15071=DIRECTION('center_axis',(1.,0.,0.));
#15072=DIRECTION('ref_axis',(0.,-3.96951249027992E-15,-1.));
#15073=DIRECTION('center_axis',(0.,-1.,0.));
#15074=DIRECTION('ref_axis',(0.,0.,-1.));
#15075=DIRECTION('',(1.,0.,0.));
#15076=DIRECTION('',(0.,0.,1.));
#15077=DIRECTION('center_axis',(1.,0.,0.));
#15078=DIRECTION('ref_axis',(0.,0.,-1.));
#15079=DIRECTION('',(0.,1.,0.));
#15080=DIRECTION('center_axis',(-1.,0.,0.));
#15081=DIRECTION('ref_axis',(0.,4.75809867696496E-16,1.));
#15082=DIRECTION('',(0.,0.,1.));
#15083=DIRECTION('center_axis',(-1.,0.,0.));
#15084=DIRECTION('ref_axis',(0.,-1.,0.));
#15085=DIRECTION('',(0.,-1.,0.));
#15086=DIRECTION('center_axis',(-1.,0.,0.));
#15087=DIRECTION('ref_axis',(0.,1.26882631385732E-15,-1.));
#15088=DIRECTION('',(0.,0.,-1.));
#15089=DIRECTION('center_axis',(-1.,0.,0.));
#15090=DIRECTION('ref_axis',(0.,1.,6.34413156928661E-16));
#15091=DIRECTION('center_axis',(0.707106781186541,0.,0.707106781186554));
#15092=DIRECTION('ref_axis',(0.707106781186554,0.,-0.707106781186541));
#15093=DIRECTION('',(0.707106781186554,3.14018491736753E-15,-0.707106781186541));
#15094=DIRECTION('',(-0.707106781186554,0.,0.707106781186541));
#15095=DIRECTION('',(0.,-1.,0.));
#15096=DIRECTION('center_axis',(-1.,0.,0.));
#15097=DIRECTION('ref_axis',(0.,4.75809867696496E-16,1.));
#15098=DIRECTION('',(0.707106781186553,0.707106781186542,0.));
#15099=DIRECTION('center_axis',(1.,0.,0.));
#15100=DIRECTION('ref_axis',(0.,4.75809867696496E-16,1.));
#15101=DIRECTION('center_axis',(0.707106781186543,-0.707106781186552,0.));
#15102=DIRECTION('ref_axis',(0.,0.,-1.));
#15103=DIRECTION('',(0.707106781186552,0.707106781186543,-6.28036983473505E-15));
#15104=DIRECTION('',(0.,0.,-1.));
#15105=DIRECTION('center_axis',(-1.,0.,0.));
#15106=DIRECTION('ref_axis',(0.,-1.,0.));
#15107=DIRECTION('',(0.707106781186554,0.,0.707106781186541));
#15108=DIRECTION('center_axis',(1.,0.,0.));
#15109=DIRECTION('ref_axis',(0.,-1.,0.));
#15110=DIRECTION('center_axis',(0.707106781186541,0.,-0.707106781186554));
#15111=DIRECTION('ref_axis',(-0.707106781186554,0.,-0.707106781186541));
#15112=DIRECTION('',(0.707106781186554,0.,0.707106781186541));
#15113=DIRECTION('',(0.,1.,0.));
#15114=DIRECTION('center_axis',(-1.,0.,0.));
#15115=DIRECTION('ref_axis',(0.,1.26882631385732E-15,-1.));
#15116=DIRECTION('',(0.70710678118656,-0.707106781186535,0.));
#15117=DIRECTION('center_axis',(1.,0.,0.));
#15118=DIRECTION('ref_axis',(0.,1.26882631385732E-15,-1.));
#15119=DIRECTION('center_axis',(0.707106781186541,0.707106781186554,0.));
#15120=DIRECTION('ref_axis',(0.,0.,-1.));
#15121=DIRECTION('',(0.707106781186554,-0.707106781186541,6.28036983473507E-15));
#15122=DIRECTION('',(0.,0.,1.));
#15123=DIRECTION('center_axis',(-1.,0.,0.));
#15124=DIRECTION('ref_axis',(0.,1.,6.34413156928661E-16));
#15125=DIRECTION('center_axis',(1.,0.,0.));
#15126=DIRECTION('ref_axis',(0.,1.,6.34413156928661E-16));
#15127=DIRECTION('center_axis',(1.,0.,0.));
#15128=DIRECTION('ref_axis',(0.,-1.,0.));
#15129=DIRECTION('',(1.,0.,0.));
#15130=DIRECTION('center_axis',(-1.,0.,0.));
#15131=DIRECTION('ref_axis',(0.,-1.,0.));
#15132=DIRECTION('',(1.,0.,0.));
#15133=DIRECTION('center_axis',(0.,-1.,0.));
#15134=DIRECTION('ref_axis',(0.,0.,-1.));
#15135=DIRECTION('',(1.,0.,0.));
#15136=DIRECTION('',(0.,0.,1.));
#15137=DIRECTION('center_axis',(1.,0.,0.));
#15138=DIRECTION('ref_axis',(0.,4.75809867696496E-16,1.));
#15139=DIRECTION('',(1.,0.,0.));
#15140=DIRECTION('center_axis',(-1.,0.,0.));
#15141=DIRECTION('ref_axis',(0.,4.75809867696496E-16,1.));
#15142=DIRECTION('center_axis',(0.,0.,1.));
#15143=DIRECTION('ref_axis',(0.,-1.,0.));
#15144=DIRECTION('',(1.,0.,0.));
#15145=DIRECTION('',(0.,1.,0.));
#15146=DIRECTION('center_axis',(-0.707106781186548,-0.707106781186547,0.));
#15147=DIRECTION('ref_axis',(0.,0.,1.));
#15148=DIRECTION('',(0.707106781186547,-0.707106781186548,5.23364152894591E-15));
#15149=DIRECTION('',(-0.707106781186547,0.707106781186548,0.));
#15150=DIRECTION('',(0.,0.,-1.));
#15151=DIRECTION('center_axis',(1.,0.,0.));
#15152=DIRECTION('ref_axis',(0.,-1.,0.));
#15153=DIRECTION('',(0.707106781186547,0.,-0.707106781186548));
#15154=DIRECTION('center_axis',(1.,0.,0.));
#15155=DIRECTION('ref_axis',(0.,-1.,0.));
#15156=DIRECTION('center_axis',(-0.707106781186548,0.,-0.707106781186547));
#15157=DIRECTION('ref_axis',(-0.707106781186547,0.,0.707106781186548));
#15158=DIRECTION('',(0.707106781186547,0.,-0.707106781186548));
#15159=DIRECTION('',(0.,-1.,0.));
#15160=DIRECTION('',(0.,1.,0.));
#15161=DIRECTION('center_axis',(1.,0.,0.));
#15162=DIRECTION('ref_axis',(0.,1.26882631385732E-15,-1.));
#15163=DIRECTION('',(0.707106781186555,0.70710678118654,0.));
#15164=DIRECTION('center_axis',(-1.,0.,0.));
#15165=DIRECTION('ref_axis',(0.,1.26882631385732E-15,-1.));
#15166=DIRECTION('center_axis',(1.,0.,0.));
#15167=DIRECTION('ref_axis',(0.,1.26882631385732E-15,-1.));
#15168=DIRECTION('center_axis',(-0.707106781186545,0.70710678118655,0.));
#15169=DIRECTION('ref_axis',(0.,0.,1.));
#15170=DIRECTION('',(0.70710678118655,0.707106781186545,-5.23364152894593E-15));
#15171=DIRECTION('',(0.,0.,-1.));
#15172=DIRECTION('',(0.,0.,1.));
#15173=DIRECTION('center_axis',(1.,0.,0.));
#15174=DIRECTION('ref_axis',(0.,1.,6.34413156928661E-16));
#15175=DIRECTION('',(0.70710678118655,0.,0.707106781186545));
#15176=DIRECTION('center_axis',(-1.,0.,0.));
#15177=DIRECTION('ref_axis',(0.,1.,6.34413156928661E-16));
#15178=DIRECTION('center_axis',(1.,0.,0.));
#15179=DIRECTION('ref_axis',(0.,1.,6.34413156928661E-16));
#15180=DIRECTION('center_axis',(-0.707106781186548,0.,0.707106781186547));
#15181=DIRECTION('ref_axis',(0.707106781186547,0.,0.707106781186548));
#15182=DIRECTION('',(0.707106781186547,-2.61682076447296E-15,0.707106781186548));
#15183=DIRECTION('',(0.,-1.,0.));
#15184=DIRECTION('center_axis',(1.,0.,0.));
#15185=DIRECTION('ref_axis',(0.,4.75809867696496E-16,1.));
#15186=DIRECTION('center_axis',(1.,0.,0.));
#15187=DIRECTION('ref_axis',(0.,4.75809867696496E-16,1.));
#15188=DIRECTION('center_axis',(1.,0.,0.));
#15189=DIRECTION('ref_axis',(0.,1.,6.34413156928661E-16));
#15190=DIRECTION('',(1.,0.,0.));
#15191=DIRECTION('center_axis',(1.,0.,0.));
#15192=DIRECTION('ref_axis',(0.,0.,-1.));
#15193=DIRECTION('',(0.,-1.,0.));
#15194=DIRECTION('center_axis',(-1.,0.,0.));
#15195=DIRECTION('ref_axis',(0.,-3.96951249027992E-15,-1.));
#15196=DIRECTION('',(0.,0.,-1.));
#15197=DIRECTION('center_axis',(-1.,0.,0.));
#15198=DIRECTION('ref_axis',(0.,1.,-5.95426873541988E-15));
#15199=DIRECTION('',(0.,1.,0.));
#15200=DIRECTION('center_axis',(-1.,0.,0.));
#15201=DIRECTION('ref_axis',(0.,-9.92378122569971E-16,1.));
#15202=DIRECTION('',(0.,0.,1.));
#15203=DIRECTION('center_axis',(-1.,0.,0.));
#15204=DIRECTION('ref_axis',(0.,-1.,-1.98475624513994E-15));
#15205=DIRECTION('center_axis',(-0.707106781186548,0.,0.707106781186547));
#15206=DIRECTION('ref_axis',(0.707106781186547,0.,0.707106781186548));
#15207=DIRECTION('',(0.707106781186547,-2.61682076447296E-15,0.707106781186548));
#15208=DIRECTION('',(-0.707106781186547,0.,-0.707106781186548));
#15209=DIRECTION('center_axis',(-1.,0.,0.));
#15210=DIRECTION('ref_axis',(0.,-1.,-1.98475624513994E-15));
#15211=DIRECTION('',(0.707106781186547,0.707106781186548,0.));
#15212=DIRECTION('center_axis',(-0.707106781186548,0.707106781186547,0.));
#15213=DIRECTION('ref_axis',(0.,0.,1.));
#15214=DIRECTION('',(0.707106781186547,0.707106781186548,0.));
#15215=DIRECTION('',(0.,0.,-1.));
#15216=DIRECTION('center_axis',(-1.,0.,0.));
#15217=DIRECTION('ref_axis',(0.,-9.92378122569971E-16,1.));
#15218=DIRECTION('',(0.707106781186547,1.30841038223648E-15,-0.707106781186548));
#15219=DIRECTION('center_axis',(1.,0.,0.));
#15220=DIRECTION('ref_axis',(0.,-9.92378122569971E-16,1.));
#15221=DIRECTION('center_axis',(-0.707106781186548,0.,-0.707106781186547));
#15222=DIRECTION('ref_axis',(-0.707106781186547,0.,0.707106781186548));
#15223=DIRECTION('',(0.707106781186545,0.,-0.70710678118655));
#15224=DIRECTION('',(0.,-1.,0.));
#15225=DIRECTION('center_axis',(-1.,0.,0.));
#15226=DIRECTION('ref_axis',(0.,1.,-5.95426873541988E-15));
#15227=DIRECTION('',(0.70710678118655,-0.707106781186545,5.23364152894593E-15));
#15228=DIRECTION('center_axis',(1.,0.,0.));
#15229=DIRECTION('ref_axis',(0.,1.,-5.95426873541988E-15));
#15230=DIRECTION('center_axis',(-0.707106781186545,-0.70710678118655,0.));
#15231=DIRECTION('ref_axis',(0.,0.,1.));
#15232=DIRECTION('',(0.70710678118655,-0.707106781186545,5.23364152894593E-15));
#15233=DIRECTION('center_axis',(-1.,0.,0.));
#15234=DIRECTION('ref_axis',(0.,-3.96951249027992E-15,-1.));
#15235=DIRECTION('center_axis',(1.,0.,0.));
#15236=DIRECTION('ref_axis',(0.,1.,-5.95426873541988E-15));
#15237=DIRECTION('',(1.,0.,0.));
#15238=DIRECTION('center_axis',(0.,0.,1.));
#15239=DIRECTION('ref_axis',(1.,0.,0.));
#15240=DIRECTION('center_axis',(0.,0.,1.));
#15241=DIRECTION('ref_axis',(1.,0.,0.));
#15242=DIRECTION('',(0.,0.,1.));
#15243=DIRECTION('center_axis',(0.,0.,-1.));
#15244=DIRECTION('ref_axis',(0.,1.,0.));
#15245=DIRECTION('',(1.,0.,0.));
#15246=DIRECTION('center_axis',(1.,0.,0.));
#15247=DIRECTION('ref_axis',(0.,-9.92378122569971E-16,1.));
#15248=DIRECTION('',(1.,0.,0.));
#15249=DIRECTION('center_axis',(0.,1.,0.));
#15250=DIRECTION('ref_axis',(0.,0.,1.));
#15251=DIRECTION('center_axis',(0.,1.,0.));
#15252=DIRECTION('ref_axis',(0.,0.,1.));
#15253=DIRECTION('',(1.,0.,0.));
#15254=DIRECTION('center_axis',(1.,0.,0.));
#15255=DIRECTION('ref_axis',(0.,1.26882631385732E-15,-1.));
#15256=DIRECTION('',(1.,0.,0.));
#15257=DIRECTION('center_axis',(0.,0.,-1.));
#15258=DIRECTION('ref_axis',(0.,1.,0.));
#15259=DIRECTION('axis',(0.,0.,1.));
#15260=DIRECTION('refdir',(1.,0.,0.));
#15261=DIRECTION('',(-0.342997170284919,8.94256168307049E-16,0.93933643662776));
#15262=DIRECTION('',(0.342997170285,-0.939336436627731,0.));
#15263=DIRECTION('',(-0.737980838656753,0.364238207643154,0.568079932640097));
#15264=DIRECTION('center_axis',(1.,0.,0.));
#15265=DIRECTION('ref_axis',(0.,-1.,0.));
#15266=DIRECTION('',(0.707106781186544,-0.352766841475276,-0.612825877028347));
#15267=DIRECTION('center_axis',(-1.,0.,0.));
#15268=DIRECTION('ref_axis',(0.,-1.,0.));
#15269=DIRECTION('',(-0.707106781186552,0.612825877028345,0.352766841475263));
#15270=DIRECTION('center_axis',(1.,0.,0.));
#15271=DIRECTION('ref_axis',(0.,-1.,0.));
#15272=DIRECTION('',(0.737980838656762,-0.568079932640111,-0.364238207643115));
#15273=DIRECTION('center_axis',(0.,0.,-1.));
#15274=DIRECTION('ref_axis',(-0.70710678118654,-0.707106781186555,0.));
#15275=DIRECTION('',(0.,0.,1.));
#15276=DIRECTION('',(0.,0.,-1.));
#15277=DIRECTION('center_axis',(0.,-1.,0.));
#15278=DIRECTION('ref_axis',(0.,0.,-1.));
#15279=DIRECTION('',(1.,0.,0.));
#15280=DIRECTION('',(-0.342997170285006,-8.94256168307127E-16,-0.939336436627728));
#15281=DIRECTION('',(0.,0.,-1.));
#15282=DIRECTION('',(0.34299717028493,-2.68276850492124E-15,-0.939336436627756));
#15283=DIRECTION('',(1.,0.,0.));
#15284=DIRECTION('',(0.342997170285008,2.6827685049214E-15,0.939336436627727));
#15285=DIRECTION('center_axis',(1.,0.,0.));
#15286=DIRECTION('ref_axis',(0.,-1.,0.));
#15287=DIRECTION('',(1.,0.,0.));
#15288=DIRECTION('center_axis',(1.,0.,0.));
#15289=DIRECTION('ref_axis',(0.,-1.,0.));
#15290=DIRECTION('',(-0.342997170284998,0.939336436627731,0.));
#15291=DIRECTION('',(-0.737980838656755,0.568079932640103,-0.364238207643142));
#15292=DIRECTION('center_axis',(1.,0.,0.));
#15293=DIRECTION('ref_axis',(0.,-1.29526019539602E-15,1.));
#15294=DIRECTION('',(0.707106781186544,-0.612825877028338,0.352766841475291));
#15295=DIRECTION('center_axis',(-1.,0.,0.));
#15296=DIRECTION('ref_axis',(0.,-1.29526019539602E-15,1.));
#15297=DIRECTION('',(-0.707106781186543,0.352766841475279,-0.612825877028346));
#15298=DIRECTION('center_axis',(1.,0.,0.));
#15299=DIRECTION('ref_axis',(0.,-1.29526019539601E-15,1.));
#15300=DIRECTION('',(0.73798083899629,-0.364238207417434,0.568079932343738));
#15301=DIRECTION('center_axis',(1.,0.,0.));
#15302=DIRECTION('ref_axis',(0.,0.,-1.));
#15303=DIRECTION('',(0.,-1.,0.));
#15304=DIRECTION('center_axis',(1.,0.,0.));
#15305=DIRECTION('ref_axis',(0.,1.,-3.7007434154172E-15));
#15306=DIRECTION('',(0.,0.,1.));
#15307=DIRECTION('center_axis',(1.,0.,0.));
#15308=DIRECTION('ref_axis',(0.,-2.96059473233375E-15,-1.));
#15309=DIRECTION('',(0.,1.,0.));
#15310=DIRECTION('',(-0.342997170285007,-0.939336436627728,0.));
#15311=DIRECTION('',(0.737980838656857,0.364238207643107,-0.568079932639993));
#15312=DIRECTION('center_axis',(-1.,0.,0.));
#15313=DIRECTION('ref_axis',(0.,-1.29526019539602E-15,1.));
#15314=DIRECTION('',(0.707106781186544,0.612825877028338,-0.352766841475291));
#15315=DIRECTION('center_axis',(-1.,0.,0.));
#15316=DIRECTION('ref_axis',(0.,-1.29526019539601E-15,1.));
#15317=DIRECTION('',(-0.707106781186543,-0.352766841475279,0.612825877028346));
#15318=DIRECTION('center_axis',(1.,0.,0.));
#15319=DIRECTION('ref_axis',(0.,-1.29526019539602E-15,1.));
#15320=DIRECTION('',(-0.737980838996349,-0.568079932343716,0.364238207417348));
#15321=DIRECTION('center_axis',(0.,0.,-1.));
#15322=DIRECTION('ref_axis',(0.70710678118654,-0.707106781186555,0.));
#15323=DIRECTION('',(0.,0.,1.));
#15324=DIRECTION('center_axis',(1.,0.,0.));
#15325=DIRECTION('ref_axis',(0.,-1.29526019539602E-15,1.));
#15326=DIRECTION('',(1.,0.,0.));
#15327=DIRECTION('',(0.342997170285021,0.939336436627723,0.));
#15328=DIRECTION('',(0.737980838996329,0.568079932343672,0.364238207417458));
#15329=DIRECTION('center_axis',(-1.,0.,0.));
#15330=DIRECTION('ref_axis',(0.,-1.,0.));
#15331=DIRECTION('',(0.707106781186544,0.352766841475276,0.612825877028347));
#15332=DIRECTION('center_axis',(-1.,0.,0.));
#15333=DIRECTION('ref_axis',(0.,-1.,0.));
#15334=DIRECTION('',(-0.707106781186552,-0.612825877028345,-0.352766841475263));
#15335=DIRECTION('',(-0.737980838656747,-0.364238207643175,-0.568079932640092));
#15336=DIRECTION('center_axis',(1.,0.,0.));
#15337=DIRECTION('ref_axis',(0.,0.,-1.));
#15338=DIRECTION('',(0.,-1.,0.));
#15339=DIRECTION('center_axis',(1.,0.,0.));
#15340=DIRECTION('ref_axis',(0.,-2.96059473233375E-15,-1.));
#15341=DIRECTION('',(0.,0.,-1.));
#15342=DIRECTION('center_axis',(1.,0.,0.));
#15343=DIRECTION('ref_axis',(0.,1.,-3.7007434154172E-15));
#15344=DIRECTION('',(0.,1.,0.));
#15345=DIRECTION('center_axis',(0.,1.,0.));
#15346=DIRECTION('ref_axis',(0.707106781186532,0.,-0.707106781186563));
#15347=DIRECTION('',(0.,1.,0.));
#15348=DIRECTION('center_axis',(1.,0.,0.));
#15349=DIRECTION('ref_axis',(0.,-2.96059473233375E-15,-1.));
#15350=DIRECTION('',(1.,0.,0.));
#15351=DIRECTION('',(1.,0.,0.));
#15352=DIRECTION('center_axis',(0.,0.,-1.));
#15353=DIRECTION('ref_axis',(0.,1.,0.));
#15354=DIRECTION('',(0.,-1.,0.));
#15355=DIRECTION('center_axis',(0.,1.,0.));
#15356=DIRECTION('ref_axis',(-0.707106781186532,0.,-0.707106781186563));
#15357=DIRECTION('center_axis',(0.,0.,1.));
#15358=DIRECTION('ref_axis',(0.707106781186532,0.707106781186563,0.));
#15359=DIRECTION('',(0.,0.,1.));
#15360=DIRECTION('center_axis',(1.,0.,0.));
#15361=DIRECTION('ref_axis',(0.,1.,-3.7007434154172E-15));
#15362=DIRECTION('',(1.,0.,0.));
#15363=DIRECTION('',(1.,0.,0.));
#15364=DIRECTION('center_axis',(0.,1.,0.));
#15365=DIRECTION('ref_axis',(0.,0.,1.));
#15366=DIRECTION('',(0.,0.,-1.));
#15367=DIRECTION('center_axis',(0.,0.,1.));
#15368=DIRECTION('ref_axis',(-0.707106781186532,0.707106781186563,0.));
#15369=DIRECTION('center_axis',(0.,-1.,0.));
#15370=DIRECTION('ref_axis',(0.70710678118654,0.,0.707106781186555));
#15371=DIRECTION('',(0.,-1.,0.));
#15372=DIRECTION('center_axis',(0.,0.,1.));
#15373=DIRECTION('ref_axis',(0.,-1.,0.));
#15374=DIRECTION('',(0.,1.,0.));
#15375=DIRECTION('center_axis',(0.,-1.,0.));
#15376=DIRECTION('ref_axis',(-0.70710678118654,0.,0.707106781186555));
#15377=DIRECTION('axis',(0.,0.,1.));
#15378=DIRECTION('refdir',(1.,0.,0.));
#15379=DIRECTION('',(-0.707106781186481,0.,0.707106781186614));
#15380=DIRECTION('',(0.707106781186525,0.,-0.70710678118657));
#15381=DIRECTION('',(-0.707106781186548,0.,0.707106781186548));
#15382=DIRECTION('center_axis',(0.707106781186548,0.,0.707106781186548));
#15383=DIRECTION('ref_axis',(0.707106781186548,0.,-0.707106781186548));
#15384=DIRECTION('',(-0.707106781186548,0.,0.707106781186548));
#15385=DIRECTION('',(0.,-1.,0.));
#15386=DIRECTION('',(0.,1.,0.));
#15387=DIRECTION('center_axis',(0.,0.,-1.));
#15388=DIRECTION('ref_axis',(0.707106781186548,0.707106781186548,0.));
#15389=DIRECTION('',(0.,0.,-1.));
#15390=DIRECTION('',(0.,0.,1.));
#15391=DIRECTION('center_axis',(1.,0.,0.));
#15392=DIRECTION('ref_axis',(0.,0.,-1.));
#15393=DIRECTION('',(0.,0.,1.));
#15394=DIRECTION('',(0.,-1.,0.));
#15395=DIRECTION('center_axis',(0.,0.,1.));
#15396=DIRECTION('ref_axis',(0.707106781186548,-0.707106781186548,0.));
#15397=DIRECTION('',(0.,0.,-1.));
#15398=DIRECTION('center_axis',(0.,1.,0.));
#15399=DIRECTION('ref_axis',(1.,0.,0.));
#15400=DIRECTION('',(1.,0.,0.));
#15401=DIRECTION('',(0.707106781186492,0.,0.707106781186603));
#15402=DIRECTION('',(0.,0.,1.));
#15403=DIRECTION('',(-0.707106781186525,0.,0.70710678118657));
#15404=DIRECTION('',(-1.,0.,0.));
#15405=DIRECTION('',(-0.707106781186481,0.,-0.707106781186614));
#15406=DIRECTION('',(0.707106781186525,0.,0.70710678118657));
#15407=DIRECTION('',(0.70710678118661,0.,0.707106781186485));
#15408=DIRECTION('center_axis',(0.707106781186548,0.,-0.707106781186548));
#15409=DIRECTION('ref_axis',(-0.707106781186548,0.,-0.707106781186548));
#15410=DIRECTION('',(0.707106781186548,0.,0.707106781186548));
#15411=DIRECTION('',(0.,1.,0.));
#15412=DIRECTION('center_axis',(-1.,0.,0.));
#15413=DIRECTION('ref_axis',(0.,0.707106781186532,-0.707106781186563));
#15414=DIRECTION('',(-1.,0.,0.));
#15415=DIRECTION('',(1.,0.,0.));
#15416=DIRECTION('center_axis',(0.,0.,-1.));
#15417=DIRECTION('ref_axis',(-1.,0.,0.));
#15418=DIRECTION('',(1.,0.,0.));
#15419=DIRECTION('',(0.,-1.,0.));
#15420=DIRECTION('center_axis',(1.,0.,0.));
#15421=DIRECTION('ref_axis',(0.,-0.707106781186532,-0.707106781186563));
#15422=DIRECTION('',(0.707106781186525,0.,-0.70710678118657));
#15423=DIRECTION('',(-0.707106781186548,0.,0.707106781186548));
#15424=DIRECTION('center_axis',(-0.707106781186548,0.,-0.707106781186548));
#15425=DIRECTION('ref_axis',(-0.707106781186548,0.,0.707106781186548));
#15426=DIRECTION('',(-0.707106781186548,0.,0.707106781186548));
#15427=DIRECTION('',(0.,1.,0.));
#15428=DIRECTION('',(-0.707106781186492,0.,-0.707106781186603));
#15429=DIRECTION('',(0.707106781186563,0.,0.707106781186532));
#15430=DIRECTION('center_axis',(-0.707106781186548,0.,0.707106781186548));
#15431=DIRECTION('ref_axis',(0.707106781186548,0.,0.707106781186548));
#15432=DIRECTION('',(0.,-1.,0.));
#15433=DIRECTION('',(0.707106781186563,0.,0.707106781186532));
#15434=DIRECTION('',(0.,1.,0.));
#15435=DIRECTION('center_axis',(0.,0.,-1.));
#15436=DIRECTION('ref_axis',(-0.707106781186563,-0.707106781186532,0.));
#15437=DIRECTION('',(0.,0.,-1.));
#15438=DIRECTION('center_axis',(-1.,0.,0.));
#15439=DIRECTION('ref_axis',(0.,0.,1.));
#15440=DIRECTION('',(0.,0.,1.));
#15441=DIRECTION('center_axis',(0.,0.,1.));
#15442=DIRECTION('ref_axis',(-0.707106781186563,0.707106781186532,0.));
#15443=DIRECTION('',(0.,0.,-1.));
#15444=DIRECTION('center_axis',(1.,0.,0.));
#15445=DIRECTION('ref_axis',(0.,0.70710678118654,0.707106781186555));
#15446=DIRECTION('',(-1.,0.,0.));
#15447=DIRECTION('',(1.,0.,0.));
#15448=DIRECTION('center_axis',(0.,1.,0.));
#15449=DIRECTION('ref_axis',(0.,0.,1.));
#15450=DIRECTION('center_axis',(-1.,0.,0.));
#15451=DIRECTION('ref_axis',(0.,-0.70710678118654,0.707106781186555));
#15452=DIRECTION('',(-1.,0.,0.));
#15453=DIRECTION('center_axis',(0.,0.,1.));
#15454=DIRECTION('ref_axis',(1.,0.,0.));
#15455=DIRECTION('axis',(0.,0.,1.));
#15456=DIRECTION('refdir',(1.,0.,0.));
#15457=DIRECTION('center_axis',(0.,0.,1.));
#15458=DIRECTION('ref_axis',(1.,0.,0.));
#15459=DIRECTION('center_axis',(0.,0.,1.));
#15460=DIRECTION('ref_axis',(1.,0.,0.));
#15461=DIRECTION('',(0.707106781186549,8.65956056235495E-17,-0.707106781186546));
#15462=DIRECTION('center_axis',(0.,0.,-1.));
#15463=DIRECTION('ref_axis',(1.,0.,0.));
#15464=DIRECTION('center_axis',(0.,0.,-1.));
#15465=DIRECTION('ref_axis',(1.,0.,0.));
#15466=DIRECTION('',(0.,0.,-1.));
#15467=DIRECTION('center_axis',(0.,0.,1.));
#15468=DIRECTION('ref_axis',(1.,0.,0.));
#15469=DIRECTION('center_axis',(0.,0.,1.));
#15470=DIRECTION('ref_axis',(-1.,0.,0.));
#15471=DIRECTION('',(1.,0.,0.));
#15472=DIRECTION('',(0.,-1.,0.));
#15473=DIRECTION('',(-1.,0.,0.));
#15474=DIRECTION('',(0.,-1.,0.));
#15475=DIRECTION('center_axis',(0.,0.,-1.));
#15476=DIRECTION('ref_axis',(1.,0.,0.));
#15477=DIRECTION('center_axis',(0.,0.,-1.));
#15478=DIRECTION('ref_axis',(1.,0.,0.));
#15479=DIRECTION('',(0.707106781186547,-8.65956056235493E-17,0.707106781186547));
#15480=DIRECTION('center_axis',(0.,0.,-1.));
#15481=DIRECTION('ref_axis',(1.,0.,0.));
#15482=DIRECTION('',(-1.,0.,0.));
#15483=DIRECTION('',(0.,-1.,0.));
#15484=DIRECTION('',(1.,0.,0.));
#15485=DIRECTION('',(0.,-1.,0.));
#15486=DIRECTION('center_axis',(0.,0.707106781186548,0.707106781186547));
#15487=DIRECTION('ref_axis',(1.,0.,0.));
#15488=DIRECTION('',(0.,0.707106781186546,-0.707106781186549));
#15489=DIRECTION('',(-1.,0.,0.));
#15490=DIRECTION('',(1.57009245868377E-15,-0.707106781186547,0.707106781186548));
#15491=DIRECTION('',(1.,0.,0.));
#15492=DIRECTION('center_axis',(0.,1.,0.));
#15493=DIRECTION('ref_axis',(1.,0.,-6.83214169000092E-15));
#15494=DIRECTION('',(0.707106781186546,0.707106781186549,-6.28036983473511E-15));
#15495=DIRECTION('center_axis',(0.,1.,0.));
#15496=DIRECTION('ref_axis',(1.,0.,-6.83214169000092E-15));
#15497=DIRECTION('center_axis',(0.,-1.,0.));
#15498=DIRECTION('ref_axis',(1.,0.,-6.83214169000092E-15));
#15499=DIRECTION('center_axis',(-0.707106781186549,0.707106781186546,0.));
#15500=DIRECTION('ref_axis',(0.,0.,1.));
#15501=DIRECTION('',(0.707106781186546,0.707106781186549,0.));
#15502=DIRECTION('',(0.,0.,-1.));
#15503=DIRECTION('',(0.,0.,1.));
#15504=DIRECTION('center_axis',(0.,1.,0.));
#15505=DIRECTION('ref_axis',(6.83214169000091E-15,0.,1.));
#15506=DIRECTION('',(6.28036983473511E-15,0.707106781186549,0.707106781186546));
#15507=DIRECTION('center_axis',(0.,1.,0.));
#15508=DIRECTION('ref_axis',(6.83214169000091E-15,0.,1.));
#15509=DIRECTION('center_axis',(0.,-1.,0.));
#15510=DIRECTION('ref_axis',(6.83214169000091E-15,0.,1.));
#15511=DIRECTION('center_axis',(0.,0.707106781186548,-0.707106781186547));
#15512=DIRECTION('ref_axis',(-1.,0.,0.));
#15513=DIRECTION('',(0.,0.707106781186547,0.707106781186548));
#15514=DIRECTION('',(1.,0.,0.));
#15515=DIRECTION('center_axis',(0.,1.,0.));
#15516=DIRECTION('ref_axis',(-1.,0.,-1.70803542250024E-15));
#15517=DIRECTION('',(-0.707106781186548,0.707106781186547,0.));
#15518=DIRECTION('center_axis',(0.,1.,0.));
#15519=DIRECTION('ref_axis',(-1.,0.,-1.70803542250024E-15));
#15520=DIRECTION('center_axis',(0.,-1.,0.));
#15521=DIRECTION('ref_axis',(-1.,0.,-1.70803542250024E-15));
#15522=DIRECTION('center_axis',(0.707106781186548,0.707106781186547,0.));
#15523=DIRECTION('ref_axis',(0.,0.,-1.));
#15524=DIRECTION('',(-0.707106781186548,0.707106781186547,0.));
#15525=DIRECTION('',(0.,0.,1.));
#15526=DIRECTION('',(0.,0.,-1.));
#15527=DIRECTION('center_axis',(0.,1.,0.));
#15528=DIRECTION('ref_axis',(0.,0.,-1.));
#15529=DIRECTION('center_axis',(0.,1.,0.));
#15530=DIRECTION('ref_axis',(0.,0.,-1.));
#15531=DIRECTION('center_axis',(0.,-1.,0.));
#15532=DIRECTION('ref_axis',(0.,0.,-1.));
#15533=DIRECTION('center_axis',(0.,-1.,0.));
#15534=DIRECTION('ref_axis',(6.83214169000091E-15,0.,1.));
#15535=DIRECTION('',(0.,-1.,0.));
#15536=DIRECTION('center_axis',(0.,1.,0.));
#15537=DIRECTION('ref_axis',(6.83214169000091E-15,0.,1.));
#15538=DIRECTION('center_axis',(-1.,0.,0.));
#15539=DIRECTION('ref_axis',(0.,0.,-1.));
#15540=DIRECTION('',(0.,-1.,0.));
#15541=DIRECTION('',(0.,0.,-1.));
#15542=DIRECTION('center_axis',(0.,-1.,0.));
#15543=DIRECTION('ref_axis',(1.,0.,-6.83214169000092E-15));
#15544=DIRECTION('',(0.,-1.,0.));
#15545=DIRECTION('center_axis',(0.,1.,0.));
#15546=DIRECTION('ref_axis',(1.,0.,-6.83214169000092E-15));
#15547=DIRECTION('center_axis',(0.,0.,1.));
#15548=DIRECTION('ref_axis',(-1.,0.,0.));
#15549=DIRECTION('',(0.,-1.,0.));
#15550=DIRECTION('',(-1.,0.,0.));
#15551=DIRECTION('center_axis',(0.,1.,0.));
#15552=DIRECTION('ref_axis',(1.,0.,0.));
#15553=DIRECTION('center_axis',(0.,-1.,0.));
#15554=DIRECTION('ref_axis',(1.97372982155583E-15,0.,1.));
#15555=DIRECTION('',(0.,0.,1.));
#15556=DIRECTION('center_axis',(0.,-1.,0.));
#15557=DIRECTION('ref_axis',(1.,0.,-1.97372982155583E-15));
#15558=DIRECTION('',(1.,0.,0.));
#15559=DIRECTION('center_axis',(0.,-1.,0.));
#15560=DIRECTION('ref_axis',(1.2335811384724E-16,0.,-1.));
#15561=DIRECTION('',(0.,0.,-1.));
#15562=DIRECTION('center_axis',(0.,-1.,0.));
#15563=DIRECTION('ref_axis',(-1.,0.,0.));
#15564=DIRECTION('',(-1.,0.,0.));
#15565=DIRECTION('center_axis',(0.,-1.,0.));
#15566=DIRECTION('ref_axis',(1.97372982155583E-15,0.,1.));
#15567=DIRECTION('',(-0.707106781186549,0.707106781186546,-3.14018491736754E-15));
#15568=DIRECTION('',(0.,-0.707106781186549,0.707106781186546));
#15569=DIRECTION('center_axis',(0.,1.,0.));
#15570=DIRECTION('ref_axis',(1.97372982155583E-15,0.,1.));
#15571=DIRECTION('center_axis',(0.707106781186549,0.707106781186546,0.));
#15572=DIRECTION('ref_axis',(0.,0.,-1.));
#15573=DIRECTION('',(0.,0.,-1.));
#15574=DIRECTION('',(-0.707106781186546,0.707106781186549,0.));
#15575=DIRECTION('center_axis',(0.,-1.,0.));
#15576=DIRECTION('ref_axis',(1.,0.,-1.97372982155583E-15));
#15577=DIRECTION('',(0.,0.707106781186549,0.707106781186546));
#15578=DIRECTION('center_axis',(0.,1.,0.));
#15579=DIRECTION('ref_axis',(1.,0.,-1.97372982155583E-15));
#15580=DIRECTION('center_axis',(0.,0.707106781186546,-0.707106781186549));
#15581=DIRECTION('ref_axis',(-1.,0.,0.));
#15582=DIRECTION('',(-1.,0.,0.));
#15583=DIRECTION('',(-7.85046229341889E-16,0.707106781186549,0.707106781186546));
#15584=DIRECTION('center_axis',(0.,-1.,0.));
#15585=DIRECTION('ref_axis',(1.2335811384724E-16,0.,-1.));
#15586=DIRECTION('',(0.707106781186547,0.707106781186548,0.));
#15587=DIRECTION('center_axis',(0.,1.,0.));
#15588=DIRECTION('ref_axis',(1.2335811384724E-16,0.,-1.));
#15589=DIRECTION('center_axis',(-0.707106781186548,0.707106781186547,0.));
#15590=DIRECTION('ref_axis',(0.,0.,1.));
#15591=DIRECTION('',(0.,0.,1.));
#15592=DIRECTION('',(0.707106781186547,0.707106781186548,0.));
#15593=DIRECTION('center_axis',(0.,-1.,0.));
#15594=DIRECTION('ref_axis',(-1.,0.,0.));
#15595=DIRECTION('',(0.,0.707106781186549,-0.707106781186546));
#15596=DIRECTION('center_axis',(0.,1.,0.));
#15597=DIRECTION('ref_axis',(-1.,0.,0.));
#15598=DIRECTION('center_axis',(0.,0.707106781186546,0.707106781186549));
#15599=DIRECTION('ref_axis',(1.,0.,0.));
#15600=DIRECTION('center_axis',(0.,0.,-1.));
#15601=DIRECTION('ref_axis',(1.,0.,0.));
#15602=DIRECTION('',(0.,-1.,0.));
#15603=DIRECTION('',(1.,0.,0.));
#15604=DIRECTION('',(0.,-1.,0.));
#15605=DIRECTION('center_axis',(0.,-1.,0.));
#15606=DIRECTION('ref_axis',(1.,0.,-1.97372982155583E-15));
#15607=DIRECTION('',(0.,-1.,0.));
#15608=DIRECTION('center_axis',(0.,-1.,0.));
#15609=DIRECTION('ref_axis',(1.,0.,-1.97372982155583E-15));
#15610=DIRECTION('center_axis',(1.,0.,0.));
#15611=DIRECTION('ref_axis',(0.,0.,1.));
#15612=DIRECTION('',(0.,-1.,0.));
#15613=DIRECTION('',(0.,0.,1.));
#15614=DIRECTION('center_axis',(0.,-1.,0.));
#15615=DIRECTION('ref_axis',(1.97372982155583E-15,0.,1.));
#15616=DIRECTION('center_axis',(0.,-1.,0.));
#15617=DIRECTION('ref_axis',(1.97372982155583E-15,0.,1.));
#15618=DIRECTION('center_axis',(0.,-0.707106781186548,-0.707106781186548));
#15619=DIRECTION('ref_axis',(-1.,0.,0.));
#15620=DIRECTION('',(0.,-0.707106781186548,0.707106781186548));
#15621=DIRECTION('',(-1.,0.,0.));
#15622=DIRECTION('',(6.54205191118239E-16,0.707106781186548,-0.707106781186548));
#15623=DIRECTION('center_axis',(0.,1.,0.));
#15624=DIRECTION('ref_axis',(1.,0.,-1.97372982155583E-15));
#15625=DIRECTION('',(-0.70710678118655,-0.707106781186545,2.61682076447295E-15));
#15626=DIRECTION('center_axis',(0.,1.,0.));
#15627=DIRECTION('ref_axis',(1.,0.,-1.97372982155583E-15));
#15628=DIRECTION('center_axis',(0.707106781186548,-0.707106781186548,0.));
#15629=DIRECTION('ref_axis',(0.,0.,-1.));
#15630=DIRECTION('',(-0.707106781186548,-0.707106781186548,2.61682076447296E-15));
#15631=DIRECTION('',(0.,0.,-1.));
#15632=DIRECTION('center_axis',(0.,1.,0.));
#15633=DIRECTION('ref_axis',(1.97372982155583E-15,0.,1.));
#15634=DIRECTION('',(0.,-0.707106781186545,-0.70710678118655));
#15635=DIRECTION('center_axis',(0.,1.,0.));
#15636=DIRECTION('ref_axis',(1.97372982155583E-15,0.,1.));
#15637=DIRECTION('center_axis',(0.,-0.707106781186548,0.707106781186548));
#15638=DIRECTION('ref_axis',(1.,0.,0.));
#15639=DIRECTION('',(-1.96261557335472E-15,-0.707106781186548,-0.707106781186548));
#15640=DIRECTION('',(1.,0.,0.));
#15641=DIRECTION('center_axis',(0.,1.,0.));
#15642=DIRECTION('ref_axis',(-1.,0.,0.));
#15643=DIRECTION('',(0.707106781186548,-0.707106781186547,0.));
#15644=DIRECTION('center_axis',(0.,1.,0.));
#15645=DIRECTION('ref_axis',(-1.,0.,0.));
#15646=DIRECTION('center_axis',(0.,-1.,0.));
#15647=DIRECTION('ref_axis',(-1.,0.,0.));
#15648=DIRECTION('center_axis',(-0.707106781186549,-0.707106781186546,0.));
#15649=DIRECTION('ref_axis',(0.,0.,1.));
#15650=DIRECTION('',(0.707106781186546,-0.707106781186549,-2.61682076447296E-15));
#15651=DIRECTION('',(0.,0.,1.));
#15652=DIRECTION('',(0.,0.,-1.));
#15653=DIRECTION('center_axis',(0.,1.,0.));
#15654=DIRECTION('ref_axis',(1.2335811384724E-16,0.,-1.));
#15655=DIRECTION('center_axis',(0.,1.,0.));
#15656=DIRECTION('ref_axis',(1.2335811384724E-16,0.,-1.));
#15657=DIRECTION('center_axis',(0.,-1.,0.));
#15658=DIRECTION('ref_axis',(1.2335811384724E-16,0.,-1.));
#15659=DIRECTION('center_axis',(0.,1.,0.));
#15660=DIRECTION('ref_axis',(1.,0.,0.));
#15661=DIRECTION('',(0.,0.,1.));
#15662=DIRECTION('center_axis',(0.,-1.,0.));
#15663=DIRECTION('ref_axis',(1.,0.,-6.83214169000092E-15));
#15664=DIRECTION('',(1.,0.,0.));
#15665=DIRECTION('center_axis',(0.,-1.,0.));
#15666=DIRECTION('ref_axis',(0.,0.,-1.));
#15667=DIRECTION('',(0.,0.,-1.));
#15668=DIRECTION('center_axis',(0.,-1.,0.));
#15669=DIRECTION('ref_axis',(-1.,0.,-1.70803542250024E-15));
#15670=DIRECTION('',(-1.,0.,0.));
#15671=DIRECTION('center_axis',(0.,-1.,0.));
#15672=DIRECTION('ref_axis',(6.83214169000091E-15,0.,1.));
#15673=DIRECTION('center_axis',(-0.707106781186548,-0.707106781186548,0.));
#15674=DIRECTION('ref_axis',(0.,0.,1.));
#15675=DIRECTION('',(0.707106781186548,-0.707106781186548,-2.61682076447296E-15));
#15676=DIRECTION('',(-0.707106781186548,0.707106781186548,0.));
#15677=DIRECTION('center_axis',(0.,-1.,0.));
#15678=DIRECTION('ref_axis',(1.,0.,-6.83214169000092E-15));
#15679=DIRECTION('',(5.23364152894591E-15,-0.707106781186548,-0.707106781186548));
#15680=DIRECTION('center_axis',(0.,-0.707106781186548,0.707106781186548));
#15681=DIRECTION('ref_axis',(1.,0.,0.));
#15682=DIRECTION('',(-1.30841038223648E-15,-0.707106781186548,-0.707106781186548));
#15683=DIRECTION('center_axis',(0.,-1.,0.));
#15684=DIRECTION('ref_axis',(0.,0.,-1.));
#15685=DIRECTION('',(-0.707106781186547,-0.707106781186548,0.));
#15686=DIRECTION('center_axis',(0.,1.,0.));
#15687=DIRECTION('ref_axis',(0.,0.,-1.));
#15688=DIRECTION('center_axis',(0.707106781186548,-0.707106781186548,0.));
#15689=DIRECTION('ref_axis',(0.,0.,-1.));
#15690=DIRECTION('',(-0.707106781186548,-0.707106781186548,2.61682076447296E-15));
#15691=DIRECTION('',(0.,0.,1.));
#15692=DIRECTION('center_axis',(0.,-1.,0.));
#15693=DIRECTION('ref_axis',(-1.,0.,-1.70803542250024E-15));
#15694=DIRECTION('',(0.,-0.707106781186548,0.707106781186548));
#15695=DIRECTION('center_axis',(0.,1.,0.));
#15696=DIRECTION('ref_axis',(-1.,0.,-1.70803542250024E-15));
#15697=DIRECTION('center_axis',(0.,-0.707106781186548,-0.707106781186548));
#15698=DIRECTION('ref_axis',(-1.,0.,0.));
#15699=DIRECTION('',(0.,-0.707106781186548,0.707106781186548));
#15700=DIRECTION('center_axis',(0.,-1.,0.));
#15701=DIRECTION('ref_axis',(6.83214169000091E-15,0.,1.));
#15702=DIRECTION('center_axis',(0.,-1.,0.));
#15703=DIRECTION('ref_axis',(0.,0.,-1.));
#15704=DIRECTION('',(0.,-1.,0.));
#15705=DIRECTION('center_axis',(0.,-1.,0.));
#15706=DIRECTION('ref_axis',(-1.,0.,-1.70803542250024E-15));
#15707=DIRECTION('',(0.,-1.,0.));
#15708=DIRECTION('center_axis',(1.,0.,0.));
#15709=DIRECTION('ref_axis',(0.,0.,1.));
#15710=DIRECTION('center_axis',(0.,-1.,0.));
#15711=DIRECTION('ref_axis',(1.2335811384724E-16,0.,-1.));
#15712=DIRECTION('',(0.,-1.,0.));
#15713=DIRECTION('center_axis',(-1.,0.,0.));
#15714=DIRECTION('ref_axis',(0.,0.,-1.));
#15715=DIRECTION('',(0.,-1.,0.));
#15716=DIRECTION('center_axis',(0.,-1.,0.));
#15717=DIRECTION('ref_axis',(-1.,0.,0.));
#15718=DIRECTION('axis',(0.,0.,1.));
#15719=DIRECTION('refdir',(1.,0.,0.));
#15720=DIRECTION('center_axis',(0.,0.,1.));
#15721=DIRECTION('ref_axis',(1.,0.,0.));
#15722=DIRECTION('center_axis',(0.,0.,1.));
#15723=DIRECTION('ref_axis',(1.,0.,0.));
#15724=DIRECTION('',(0.707106781186547,8.65956056235493E-17,-0.707106781186547));
#15725=DIRECTION('center_axis',(0.,0.,-1.));
#15726=DIRECTION('ref_axis',(1.,0.,0.));
#15727=DIRECTION('center_axis',(0.,0.,1.));
#15728=DIRECTION('ref_axis',(0.,-1.,0.));
#15729=DIRECTION('',(0.,1.,0.));
#15730=DIRECTION('',(1.,0.,0.));
#15731=DIRECTION('',(0.,-1.,0.));
#15732=DIRECTION('',(1.,0.,0.));
#15733=DIRECTION('center_axis',(0.,0.,1.));
#15734=DIRECTION('ref_axis',(1.,0.,0.));
#15735=DIRECTION('center_axis',(0.,0.,1.));
#15736=DIRECTION('ref_axis',(1.,0.,0.));
#15737=DIRECTION('center_axis',(0.,0.,1.));
#15738=DIRECTION('ref_axis',(1.,0.,0.));
#15739=DIRECTION('center_axis',(0.,0.,1.));
#15740=DIRECTION('ref_axis',(1.,0.,0.));
#15741=DIRECTION('center_axis',(0.,0.,1.));
#15742=DIRECTION('ref_axis',(1.,0.,0.));
#15743=DIRECTION('center_axis',(0.,0.,1.));
#15744=DIRECTION('ref_axis',(1.,0.,0.));
#15745=DIRECTION('center_axis',(0.,0.,1.));
#15746=DIRECTION('ref_axis',(1.,0.,0.));
#15747=DIRECTION('',(0.,0.,1.));
#15748=DIRECTION('center_axis',(0.,0.,1.));
#15749=DIRECTION('ref_axis',(1.,0.,0.));
#15750=DIRECTION('',(0.707106781186549,8.65956056235495E-17,-0.707106781186546));
#15751=DIRECTION('center_axis',(0.,0.,-1.));
#15752=DIRECTION('ref_axis',(1.,0.,0.));
#15753=DIRECTION('center_axis',(0.,0.,1.));
#15754=DIRECTION('ref_axis',(1.,0.,0.));
#15755=DIRECTION('center_axis',(0.,0.,1.));
#15756=DIRECTION('ref_axis',(1.,0.,0.));
#15757=DIRECTION('',(0.,0.,1.));
#15758=DIRECTION('center_axis',(0.,0.,1.));
#15759=DIRECTION('ref_axis',(1.,0.,0.));
#15760=DIRECTION('',(0.707106781186549,8.65956056235495E-17,-0.707106781186546));
#15761=DIRECTION('center_axis',(0.,0.,-1.));
#15762=DIRECTION('ref_axis',(1.,0.,0.));
#15763=DIRECTION('center_axis',(0.,0.,1.));
#15764=DIRECTION('ref_axis',(1.,0.,0.));
#15765=DIRECTION('center_axis',(0.,0.,1.));
#15766=DIRECTION('ref_axis',(1.,0.,0.));
#15767=DIRECTION('',(0.,0.,1.));
#15768=DIRECTION('center_axis',(0.,0.,1.));
#15769=DIRECTION('ref_axis',(1.,0.,0.));
#15770=DIRECTION('',(0.707106781186548,8.65956056235493E-17,-0.707106781186548));
#15771=DIRECTION('center_axis',(0.,0.,-1.));
#15772=DIRECTION('ref_axis',(1.,0.,0.));
#15773=DIRECTION('center_axis',(0.,0.,1.));
#15774=DIRECTION('ref_axis',(1.,0.,0.));
#15775=DIRECTION('center_axis',(0.,0.,1.));
#15776=DIRECTION('ref_axis',(1.,0.,0.));
#15777=DIRECTION('',(0.,0.,1.));
#15778=DIRECTION('center_axis',(0.,0.,1.));
#15779=DIRECTION('ref_axis',(1.,0.,0.));
#15780=DIRECTION('',(0.707106781186547,8.65956056235493E-17,-0.707106781186547));
#15781=DIRECTION('center_axis',(0.,0.,-1.));
#15782=DIRECTION('ref_axis',(1.,0.,0.));
#15783=DIRECTION('center_axis',(0.,0.,1.));
#15784=DIRECTION('ref_axis',(1.,0.,0.));
#15785=DIRECTION('center_axis',(0.,0.,1.));
#15786=DIRECTION('ref_axis',(1.,0.,0.));
#15787=DIRECTION('',(0.,0.,1.));
#15788=DIRECTION('center_axis',(0.,0.,1.));
#15789=DIRECTION('ref_axis',(1.,0.,0.));
#15790=DIRECTION('',(0.707106781186547,8.65956056235493E-17,-0.707106781186547));
#15791=DIRECTION('center_axis',(0.,0.,-1.));
#15792=DIRECTION('ref_axis',(1.,0.,0.));
#15793=DIRECTION('center_axis',(0.,0.,1.));
#15794=DIRECTION('ref_axis',(1.,0.,0.));
#15795=DIRECTION('center_axis',(0.,0.,1.));
#15796=DIRECTION('ref_axis',(1.,0.,0.));
#15797=DIRECTION('',(0.,0.,1.));
#15798=DIRECTION('center_axis',(0.,1.,0.));
#15799=DIRECTION('ref_axis',(1.,0.,0.));
#15800=DIRECTION('center_axis',(0.,1.,0.));
#15801=DIRECTION('ref_axis',(1.,0.,0.));
#15802=DIRECTION('',(0.707106781186546,-0.707106781186549,-8.65956056235491E-17));
#15803=DIRECTION('center_axis',(0.,-1.,0.));
#15804=DIRECTION('ref_axis',(1.,0.,0.));
#15805=DIRECTION('center_axis',(0.,1.,0.));
#15806=DIRECTION('ref_axis',(0.,0.,1.));
#15807=DIRECTION('',(0.,0.,-1.));
#15808=DIRECTION('',(1.,0.,0.));
#15809=DIRECTION('',(0.,0.,1.));
#15810=DIRECTION('',(1.,0.,0.));
#15811=DIRECTION('center_axis',(0.,1.,0.));
#15812=DIRECTION('ref_axis',(1.,0.,0.));
#15813=DIRECTION('center_axis',(0.,1.,0.));
#15814=DIRECTION('ref_axis',(1.,0.,0.));
#15815=DIRECTION('center_axis',(0.,1.,0.));
#15816=DIRECTION('ref_axis',(1.,0.,0.));
#15817=DIRECTION('center_axis',(0.,1.,0.));
#15818=DIRECTION('ref_axis',(1.,0.,0.));
#15819=DIRECTION('center_axis',(0.,1.,0.));
#15820=DIRECTION('ref_axis',(1.,0.,0.));
#15821=DIRECTION('center_axis',(0.,1.,0.));
#15822=DIRECTION('ref_axis',(1.,0.,0.));
#15823=DIRECTION('center_axis',(0.,1.,0.));
#15824=DIRECTION('ref_axis',(1.,0.,0.));
#15825=DIRECTION('center_axis',(0.,1.,0.));
#15826=DIRECTION('ref_axis',(1.,0.,0.));
#15827=DIRECTION('',(0.,1.,0.));
#15828=DIRECTION('center_axis',(-0.707106781186548,0.707106781186548,0.));
#15829=DIRECTION('ref_axis',(0.,0.,1.));
#15830=DIRECTION('',(0.707106781186548,0.707106781186548,-3.14018491736756E-15));
#15831=DIRECTION('',(-0.707106781186548,-0.707106781186548,0.));
#15832=DIRECTION('',(0.,0.,1.));
#15833=DIRECTION('center_axis',(-1.,0.,0.));
#15834=DIRECTION('ref_axis',(0.,1.79429983777803E-15,1.));
#15835=DIRECTION('',(0.707106781186548,0.,-0.707106781186548));
#15836=DIRECTION('center_axis',(1.,0.,0.));
#15837=DIRECTION('ref_axis',(0.,1.79429983777803E-15,1.));
#15838=DIRECTION('center_axis',(-1.,0.,0.));
#15839=DIRECTION('ref_axis',(0.,1.79429983777803E-15,1.));
#15840=DIRECTION('center_axis',(-0.707106781186548,0.,-0.707106781186548));
#15841=DIRECTION('ref_axis',(-0.707106781186548,0.,0.707106781186548));
#15842=DIRECTION('',(0.707106781186541,0.,-0.707106781186554));
#15843=DIRECTION('',(0.,-1.,0.));
#15844=DIRECTION('',(0.,1.,0.));
#15845=DIRECTION('center_axis',(-1.,0.,0.));
#15846=DIRECTION('ref_axis',(0.,1.,1.79429983777804E-15));
#15847=DIRECTION('',(0.707106781186548,-0.707106781186548,0.));
#15848=DIRECTION('center_axis',(1.,0.,0.));
#15849=DIRECTION('ref_axis',(0.,1.,1.79429983777804E-15));
#15850=DIRECTION('center_axis',(-1.,0.,0.));
#15851=DIRECTION('ref_axis',(0.,1.,1.79429983777804E-15));
#15852=DIRECTION('center_axis',(-0.707106781186548,-0.707106781186548,0.));
#15853=DIRECTION('ref_axis',(0.,0.,1.));
#15854=DIRECTION('',(0.707106781186554,-0.707106781186541,3.14018491736759E-15));
#15855=DIRECTION('',(0.,0.,1.));
#15856=DIRECTION('',(0.,0.,-1.));
#15857=DIRECTION('center_axis',(-1.,0.,0.));
#15858=DIRECTION('ref_axis',(0.,-7.17719935111212E-15,-1.));
#15859=DIRECTION('',(0.707106781186548,0.,0.707106781186548));
#15860=DIRECTION('center_axis',(1.,0.,0.));
#15861=DIRECTION('ref_axis',(0.,-7.17719935111212E-15,-1.));
#15862=DIRECTION('center_axis',(-1.,0.,0.));
#15863=DIRECTION('ref_axis',(0.,-7.17719935111212E-15,-1.));
#15864=DIRECTION('center_axis',(-0.707106781186548,0.,0.707106781186548));
#15865=DIRECTION('ref_axis',(0.707106781186548,0.,0.707106781186548));
#15866=DIRECTION('',(0.707106781186548,-3.14018491736756E-15,0.707106781186548));
#15867=DIRECTION('',(0.,-1.,0.));
#15868=DIRECTION('center_axis',(-1.,0.,0.));
#15869=DIRECTION('ref_axis',(0.,-1.,0.));
#15870=DIRECTION('center_axis',(1.,0.,0.));
#15871=DIRECTION('ref_axis',(0.,-1.,0.));
#15872=DIRECTION('center_axis',(-1.,0.,0.));
#15873=DIRECTION('ref_axis',(0.,-1.,0.));
#15874=DIRECTION('center_axis',(1.,0.,0.));
#15875=DIRECTION('ref_axis',(0.,-7.17719935111212E-15,-1.));
#15876=DIRECTION('center_axis',(-1.,0.,0.));
#15877=DIRECTION('ref_axis',(0.,-7.17719935111212E-15,-1.));
#15878=DIRECTION('',(1.,0.,0.));
#15879=DIRECTION('center_axis',(1.,0.,0.));
#15880=DIRECTION('ref_axis',(0.,-1.,0.));
#15881=DIRECTION('center_axis',(-1.,0.,0.));
#15882=DIRECTION('ref_axis',(0.,-1.,0.));
#15883=DIRECTION('center_axis',(1.,0.,0.));
#15884=DIRECTION('ref_axis',(0.,0.,-1.));
#15885=DIRECTION('',(0.,1.,0.));
#15886=DIRECTION('center_axis',(1.,0.,0.));
#15887=DIRECTION('ref_axis',(0.,-1.,-1.48029736616687E-15));
#15888=DIRECTION('',(0.,0.,-1.));
#15889=DIRECTION('center_axis',(1.,0.,0.));
#15890=DIRECTION('ref_axis',(0.,-1.85037170770859E-15,1.));
#15891=DIRECTION('',(0.,-1.,0.));
#15892=DIRECTION('center_axis',(1.,0.,0.));
#15893=DIRECTION('ref_axis',(0.,1.,2.22044604925031E-15));
#15894=DIRECTION('',(0.,0.,1.));
#15895=DIRECTION('center_axis',(1.,0.,0.));
#15896=DIRECTION('ref_axis',(0.,2.96059473233374E-15,-1.));
#15897=DIRECTION('center_axis',(0.,1.,0.));
#15898=DIRECTION('ref_axis',(1.,0.,0.));
#15899=DIRECTION('',(0.707106781186546,-0.707106781186549,-8.65956056235492E-17));
#15900=DIRECTION('center_axis',(0.,-1.,0.));
#15901=DIRECTION('ref_axis',(1.,0.,0.));
#15902=DIRECTION('center_axis',(0.,1.,0.));
#15903=DIRECTION('ref_axis',(1.,0.,0.));
#15904=DIRECTION('center_axis',(0.,1.,0.));
#15905=DIRECTION('ref_axis',(1.,0.,0.));
#15906=DIRECTION('',(0.,1.,0.));
#15907=DIRECTION('center_axis',(0.,1.,0.));
#15908=DIRECTION('ref_axis',(1.,0.,0.));
#15909=DIRECTION('',(0.707106781186546,-0.707106781186549,-8.65956056235491E-17));
#15910=DIRECTION('center_axis',(0.,-1.,0.));
#15911=DIRECTION('ref_axis',(1.,0.,0.));
#15912=DIRECTION('center_axis',(0.,1.,0.));
#15913=DIRECTION('ref_axis',(1.,0.,0.));
#15914=DIRECTION('center_axis',(0.,1.,0.));
#15915=DIRECTION('ref_axis',(1.,0.,0.));
#15916=DIRECTION('',(0.,1.,0.));
#15917=DIRECTION('center_axis',(0.,1.,0.));
#15918=DIRECTION('ref_axis',(1.,0.,0.));
#15919=DIRECTION('',(0.707106781186546,-0.707106781186549,-8.65956056235491E-17));
#15920=DIRECTION('center_axis',(0.,-1.,0.));
#15921=DIRECTION('ref_axis',(1.,0.,0.));
#15922=DIRECTION('center_axis',(0.,1.,0.));
#15923=DIRECTION('ref_axis',(1.,0.,0.));
#15924=DIRECTION('center_axis',(0.,1.,0.));
#15925=DIRECTION('ref_axis',(1.,0.,0.));
#15926=DIRECTION('',(0.,1.,0.));
#15927=DIRECTION('center_axis',(0.,1.,0.));
#15928=DIRECTION('ref_axis',(1.,0.,0.));
#15929=DIRECTION('',(0.707106781186547,-0.707106781186547,-8.65956056235493E-17));
#15930=DIRECTION('center_axis',(0.,-1.,0.));
#15931=DIRECTION('ref_axis',(1.,0.,0.));
#15932=DIRECTION('center_axis',(0.,1.,0.));
#15933=DIRECTION('ref_axis',(1.,0.,0.));
#15934=DIRECTION('center_axis',(0.,1.,0.));
#15935=DIRECTION('ref_axis',(1.,0.,0.));
#15936=DIRECTION('',(0.,1.,0.));
#15937=DIRECTION('center_axis',(0.,1.,0.));
#15938=DIRECTION('ref_axis',(1.,0.,0.));
#15939=DIRECTION('',(0.707106781186547,-0.707106781186547,-8.65956056235493E-17));
#15940=DIRECTION('center_axis',(0.,-1.,0.));
#15941=DIRECTION('ref_axis',(1.,0.,0.));
#15942=DIRECTION('center_axis',(0.,1.,0.));
#15943=DIRECTION('ref_axis',(1.,0.,0.));
#15944=DIRECTION('center_axis',(0.,1.,0.));
#15945=DIRECTION('ref_axis',(1.,0.,0.));
#15946=DIRECTION('',(0.,1.,0.));
#15947=DIRECTION('center_axis',(0.,1.,0.));
#15948=DIRECTION('ref_axis',(1.,0.,0.));
#15949=DIRECTION('',(0.707106781186546,-0.707106781186549,-8.65956056235491E-17));
#15950=DIRECTION('center_axis',(0.,-1.,0.));
#15951=DIRECTION('ref_axis',(1.,0.,0.));
#15952=DIRECTION('center_axis',(0.,1.,0.));
#15953=DIRECTION('ref_axis',(1.,0.,0.));
#15954=DIRECTION('center_axis',(0.,1.,0.));
#15955=DIRECTION('ref_axis',(1.,0.,0.));
#15956=DIRECTION('',(0.,1.,0.));
#15957=DIRECTION('center_axis',(0.,-1.,0.));
#15958=DIRECTION('ref_axis',(1.,0.,0.));
#15959=DIRECTION('center_axis',(0.,-1.,0.));
#15960=DIRECTION('ref_axis',(1.,0.,0.));
#15961=DIRECTION('',(0.707106781186546,0.707106781186549,8.65956056235492E-17));
#15962=DIRECTION('center_axis',(0.,-1.,0.));
#15963=DIRECTION('ref_axis',(0.,0.,-1.));
#15964=DIRECTION('',(0.,0.,1.));
#15965=DIRECTION('',(1.,0.,0.));
#15966=DIRECTION('',(0.,0.,-1.));
#15967=DIRECTION('',(1.,0.,0.));
#15968=DIRECTION('center_axis',(0.,-1.,0.));
#15969=DIRECTION('ref_axis',(1.,0.,0.));
#15970=DIRECTION('center_axis',(0.,-1.,0.));
#15971=DIRECTION('ref_axis',(1.,0.,0.));
#15972=DIRECTION('center_axis',(0.,-1.,0.));
#15973=DIRECTION('ref_axis',(1.,0.,0.));
#15974=DIRECTION('center_axis',(0.,-1.,0.));
#15975=DIRECTION('ref_axis',(1.,0.,0.));
#15976=DIRECTION('center_axis',(0.,-1.,0.));
#15977=DIRECTION('ref_axis',(1.,0.,0.));
#15978=DIRECTION('center_axis',(0.,-1.,0.));
#15979=DIRECTION('ref_axis',(1.,0.,0.));
#15980=DIRECTION('center_axis',(0.,-1.,0.));
#15981=DIRECTION('ref_axis',(1.,0.,0.));
#15982=DIRECTION('',(0.707106781186546,0.707106781186549,8.65956056235491E-17));
#15983=DIRECTION('center_axis',(0.,-1.,0.));
#15984=DIRECTION('ref_axis',(1.,0.,0.));
#15985=DIRECTION('',(0.707106781186546,0.707106781186549,8.65956056235491E-17));
#15986=DIRECTION('center_axis',(0.,-1.,0.));
#15987=DIRECTION('ref_axis',(1.,0.,0.));
#15988=DIRECTION('',(0.707106781186546,0.707106781186549,8.65956056235491E-17));
#15989=DIRECTION('center_axis',(0.,-1.,0.));
#15990=DIRECTION('ref_axis',(1.,0.,0.));
#15991=DIRECTION('',(0.707106781186547,0.707106781186547,8.65956056235493E-17));
#15992=DIRECTION('center_axis',(0.,-1.,0.));
#15993=DIRECTION('ref_axis',(1.,0.,0.));
#15994=DIRECTION('',(0.707106781186547,0.707106781186547,8.65956056235493E-17));
#15995=DIRECTION('center_axis',(0.,-1.,0.));
#15996=DIRECTION('ref_axis',(1.,0.,0.));
#15997=DIRECTION('',(0.707106781186546,0.707106781186549,8.65956056235491E-17));
#15998=DIRECTION('center_axis',(-0.707106781186548,0.,-0.707106781186548));
#15999=DIRECTION('ref_axis',(-0.707106781186548,0.,0.707106781186548));
#16000=DIRECTION('',(0.707106781186548,0.,-0.707106781186548));
#16001=DIRECTION('',(0.,-1.,0.));
#16002=DIRECTION('',(-0.707106781186548,0.,0.707106781186548));
#16003=DIRECTION('center_axis',(1.,0.,0.));
#16004=DIRECTION('ref_axis',(0.,2.96059473233374E-15,-1.));
#16005=DIRECTION('',(0.707106781186548,0.707106781186548,0.));
#16006=DIRECTION('center_axis',(-1.,0.,0.));
#16007=DIRECTION('ref_axis',(0.,2.96059473233374E-15,-1.));
#16008=DIRECTION('center_axis',(-0.707106781186548,0.707106781186548,0.));
#16009=DIRECTION('ref_axis',(0.,0.,1.));
#16010=DIRECTION('',(0.707106781186548,0.707106781186548,-3.14018491736756E-15));
#16011=DIRECTION('',(0.,0.,-1.));
#16012=DIRECTION('center_axis',(1.,0.,0.));
#16013=DIRECTION('ref_axis',(0.,1.,2.22044604925031E-15));
#16014=DIRECTION('',(0.707106781186548,0.,0.707106781186548));
#16015=DIRECTION('center_axis',(-1.,0.,0.));
#16016=DIRECTION('ref_axis',(0.,1.,2.22044604925031E-15));
#16017=DIRECTION('center_axis',(-0.707106781186548,0.,0.707106781186548));
#16018=DIRECTION('ref_axis',(0.707106781186548,0.,0.707106781186548));
#16019=DIRECTION('',(0.707106781186548,-3.14018491736756E-15,0.707106781186548));
#16020=DIRECTION('',(0.,1.,0.));
#16021=DIRECTION('center_axis',(1.,0.,0.));
#16022=DIRECTION('ref_axis',(0.,-1.85037170770859E-15,1.));
#16023=DIRECTION('',(0.707106781186546,-0.707106781186549,3.14018491736755E-15));
#16024=DIRECTION('center_axis',(-1.,0.,0.));
#16025=DIRECTION('ref_axis',(0.,-1.85037170770859E-15,1.));
#16026=DIRECTION('center_axis',(-0.707106781186548,-0.707106781186547,0.));
#16027=DIRECTION('ref_axis',(0.,0.,1.));
#16028=DIRECTION('',(0.707106781186547,-0.707106781186548,3.14018491736756E-15));
#16029=DIRECTION('center_axis',(1.,0.,0.));
#16030=DIRECTION('ref_axis',(0.,-1.,-1.48029736616687E-15));
#16031=DIRECTION('center_axis',(-1.,0.,0.));
#16032=DIRECTION('ref_axis',(0.,-1.,-1.48029736616687E-15));
#16033=DIRECTION('center_axis',(1.,0.,0.));
#16034=DIRECTION('ref_axis',(0.,-1.85037170770859E-15,1.));
#16035=DIRECTION('center_axis',(1.,0.,0.));
#16036=DIRECTION('ref_axis',(0.,-1.85037170770859E-15,1.));
#16037=DIRECTION('',(1.,0.,0.));
#16038=DIRECTION('center_axis',(1.,0.,0.));
#16039=DIRECTION('ref_axis',(0.,-1.,-1.48029736616687E-15));
#16040=DIRECTION('',(1.,0.,0.));
#16041=DIRECTION('center_axis',(1.,0.,0.));
#16042=DIRECTION('ref_axis',(0.,-1.,-1.48029736616687E-15));
#16043=DIRECTION('center_axis',(0.,0.,-1.));
#16044=DIRECTION('ref_axis',(0.,1.,0.));
#16045=DIRECTION('',(1.,0.,0.));
#16046=DIRECTION('',(0.,1.,0.));
#16047=DIRECTION('center_axis',(0.,0.,-1.));
#16048=DIRECTION('ref_axis',(1.,0.,0.));
#16049=DIRECTION('center_axis',(0.,0.,-1.));
#16050=DIRECTION('ref_axis',(1.,0.,0.));
#16051=DIRECTION('center_axis',(0.,0.,-1.));
#16052=DIRECTION('ref_axis',(1.,0.,0.));
#16053=DIRECTION('center_axis',(0.,0.,-1.));
#16054=DIRECTION('ref_axis',(1.,0.,0.));
#16055=DIRECTION('center_axis',(0.,0.,-1.));
#16056=DIRECTION('ref_axis',(1.,0.,0.));
#16057=DIRECTION('center_axis',(0.,0.,-1.));
#16058=DIRECTION('ref_axis',(1.,0.,0.));
#16059=DIRECTION('center_axis',(0.,0.,-1.));
#16060=DIRECTION('ref_axis',(1.,0.,0.));
#16061=DIRECTION('',(0.707106781186547,-8.65956056235493E-17,0.707106781186547));
#16062=DIRECTION('center_axis',(0.,0.,-1.));
#16063=DIRECTION('ref_axis',(1.,0.,0.));
#16064=DIRECTION('',(0.707106781186547,-8.65956056235493E-17,0.707106781186547));
#16065=DIRECTION('center_axis',(0.,0.,-1.));
#16066=DIRECTION('ref_axis',(1.,0.,0.));
#16067=DIRECTION('',(0.707106781186548,-8.65956056235493E-17,0.707106781186548));
#16068=DIRECTION('center_axis',(0.,0.,-1.));
#16069=DIRECTION('ref_axis',(1.,0.,0.));
#16070=DIRECTION('',(0.707106781186549,-8.65956056235495E-17,0.707106781186546));
#16071=DIRECTION('center_axis',(0.,0.,-1.));
#16072=DIRECTION('ref_axis',(1.,0.,0.));
#16073=DIRECTION('',(0.707106781186549,-8.65956056235495E-17,0.707106781186546));
#16074=DIRECTION('center_axis',(0.,0.,-1.));
#16075=DIRECTION('ref_axis',(1.,0.,0.));
#16076=DIRECTION('',(0.707106781186547,-8.65956056235493E-17,0.707106781186547));
#16077=DIRECTION('center_axis',(0.707106781186534,-0.707106781186561,0.));
#16078=DIRECTION('ref_axis',(0.,0.,-1.));
#16079=DIRECTION('',(0.707106781186561,0.707106781186534,-2.61682076447291E-15));
#16080=DIRECTION('',(0.,0.,1.));
#16081=DIRECTION('',(-0.707106781186563,-0.707106781186532,0.));
#16082=DIRECTION('center_axis',(-1.,0.,0.));
#16083=DIRECTION('ref_axis',(0.,-1.,-1.48029736616687E-15));
#16084=DIRECTION('',(0.707106781186561,2.61682076447291E-15,0.707106781186534));
#16085=DIRECTION('center_axis',(-1.,0.,0.));
#16086=DIRECTION('ref_axis',(0.,-1.,-1.48029736616687E-15));
#16087=DIRECTION('center_axis',(0.707106781186534,0.,-0.707106781186561));
#16088=DIRECTION('ref_axis',(-0.707106781186561,0.,-0.707106781186534));
#16089=DIRECTION('',(0.707106781186561,0.,0.707106781186534));
#16090=DIRECTION('',(0.,-1.,0.));
#16091=DIRECTION('center_axis',(-1.,0.,0.));
#16092=DIRECTION('ref_axis',(0.,2.96059473233374E-15,-1.));
#16093=DIRECTION('',(0.707106781186563,-0.707106781186532,0.));
#16094=DIRECTION('center_axis',(-1.,0.,0.));
#16095=DIRECTION('ref_axis',(0.,2.96059473233374E-15,-1.));
#16096=DIRECTION('center_axis',(1.,0.,0.));
#16097=DIRECTION('ref_axis',(0.,2.96059473233374E-15,-1.));
#16098=DIRECTION('center_axis',(0.707106781186532,0.707106781186563,0.));
#16099=DIRECTION('ref_axis',(0.,0.,-1.));
#16100=DIRECTION('',(0.707106781186563,-0.707106781186532,2.61682076447292E-15));
#16101=DIRECTION('',(0.,0.,-1.));
#16102=DIRECTION('',(0.,0.,1.));
#16103=DIRECTION('center_axis',(-1.,0.,0.));
#16104=DIRECTION('ref_axis',(0.,1.,2.22044604925031E-15));
#16105=DIRECTION('',(0.707106781186563,0.,-0.707106781186532));
#16106=DIRECTION('center_axis',(-1.,0.,0.));
#16107=DIRECTION('ref_axis',(0.,1.,2.22044604925031E-15));
#16108=DIRECTION('center_axis',(1.,0.,0.));
#16109=DIRECTION('ref_axis',(0.,1.,2.22044604925031E-15));
#16110=DIRECTION('center_axis',(0.707106781186534,0.,0.707106781186561));
#16111=DIRECTION('ref_axis',(0.707106781186561,0.,-0.707106781186534));
#16112=DIRECTION('',(0.707106781186561,2.61682076447291E-15,-0.707106781186534));
#16113=DIRECTION('',(0.,1.,0.));
#16114=DIRECTION('',(0.,-1.,0.));
#16115=DIRECTION('center_axis',(-1.,0.,0.));
#16116=DIRECTION('ref_axis',(0.,-1.85037170770859E-15,1.));
#16117=DIRECTION('center_axis',(-1.,0.,0.));
#16118=DIRECTION('ref_axis',(0.,-1.85037170770859E-15,1.));
#16119=DIRECTION('center_axis',(1.,0.,0.));
#16120=DIRECTION('ref_axis',(0.,2.96059473233374E-15,-1.));
#16121=DIRECTION('',(1.,0.,0.));
#16122=DIRECTION('center_axis',(1.,0.,0.));
#16123=DIRECTION('ref_axis',(0.,0.,-1.));
#16124=DIRECTION('',(0.,1.,0.));
#16125=DIRECTION('center_axis',(1.,0.,0.));
#16126=DIRECTION('ref_axis',(0.,-1.,0.));
#16127=DIRECTION('',(0.,0.,-1.));
#16128=DIRECTION('center_axis',(1.,0.,0.));
#16129=DIRECTION('ref_axis',(0.,1.79429983777803E-15,1.));
#16130=DIRECTION('',(0.,-1.,0.));
#16131=DIRECTION('center_axis',(1.,0.,0.));
#16132=DIRECTION('ref_axis',(0.,1.,1.79429983777804E-15));
#16133=DIRECTION('',(0.,0.,1.));
#16134=DIRECTION('center_axis',(1.,0.,0.));
#16135=DIRECTION('ref_axis',(0.,-7.17719935111212E-15,-1.));
#16136=DIRECTION('center_axis',(0.707106781186534,0.,0.707106781186561));
#16137=DIRECTION('ref_axis',(0.707106781186561,0.,-0.707106781186534));
#16138=DIRECTION('',(0.707106781186561,2.61682076447291E-15,-0.707106781186534));
#16139=DIRECTION('',(-0.707106781186561,0.,0.707106781186534));
#16140=DIRECTION('center_axis',(1.,0.,0.));
#16141=DIRECTION('ref_axis',(0.,-1.,0.));
#16142=DIRECTION('',(0.707106781186561,-0.707106781186534,0.));
#16143=DIRECTION('center_axis',(0.707106781186534,0.707106781186561,0.));
#16144=DIRECTION('ref_axis',(0.,0.,-1.));
#16145=DIRECTION('',(0.707106781186561,-0.707106781186534,2.61682076447291E-15));
#16146=DIRECTION('center_axis',(1.,0.,0.));
#16147=DIRECTION('ref_axis',(0.,1.79429983777803E-15,1.));
#16148=DIRECTION('',(0.707106781186561,0.,0.707106781186534));
#16149=DIRECTION('center_axis',(-1.,0.,0.));
#16150=DIRECTION('ref_axis',(0.,1.79429983777803E-15,1.));
#16151=DIRECTION('center_axis',(0.707106781186534,0.,-0.707106781186561));
#16152=DIRECTION('ref_axis',(-0.707106781186561,0.,-0.707106781186534));
#16153=DIRECTION('',(0.707106781186555,0.,0.70710678118654));
#16154=DIRECTION('',(0.,1.,0.));
#16155=DIRECTION('center_axis',(1.,0.,0.));
#16156=DIRECTION('ref_axis',(0.,1.,1.79429983777804E-15));
#16157=DIRECTION('',(0.707106781186563,0.707106781186532,0.));
#16158=DIRECTION('center_axis',(-1.,0.,0.));
#16159=DIRECTION('ref_axis',(0.,1.,1.79429983777804E-15));
#16160=DIRECTION('center_axis',(0.707106781186532,-0.707106781186563,0.));
#16161=DIRECTION('ref_axis',(0.,0.,-1.));
#16162=DIRECTION('',(0.707106781186568,0.707106781186527,-2.61682076447294E-15));
#16163=DIRECTION('',(0.,0.,-1.));
#16164=DIRECTION('center_axis',(1.,0.,0.));
#16165=DIRECTION('ref_axis',(0.,-7.17719935111212E-15,-1.));
#16166=DIRECTION('center_axis',(1.,0.,0.));
#16167=DIRECTION('ref_axis',(0.,1.79429983777803E-15,1.));
#16168=DIRECTION('',(1.,0.,0.));
#16169=DIRECTION('center_axis',(0.,-1.,0.));
#16170=DIRECTION('ref_axis',(0.,0.,-1.));
#16171=DIRECTION('',(1.,0.,0.));
#16172=DIRECTION('center_axis',(1.,0.,0.));
#16173=DIRECTION('ref_axis',(0.,1.,1.79429983777804E-15));
#16174=DIRECTION('',(1.,0.,0.));
#16175=DIRECTION('center_axis',(0.,0.,-1.));
#16176=DIRECTION('ref_axis',(0.,1.,0.));
#16177=DIRECTION('center_axis',(0.,0.,1.));
#16178=DIRECTION('ref_axis',(0.,-1.,0.));
#16179=DIRECTION('',(1.,0.,0.));
#16180=DIRECTION('center_axis',(1.,0.,0.));
#16181=DIRECTION('ref_axis',(0.,1.,2.22044604925031E-15));
#16182=DIRECTION('',(1.,0.,0.));
#16183=DIRECTION('center_axis',(0.,1.,0.));
#16184=DIRECTION('ref_axis',(0.,0.,1.));
#16185=DIRECTION('axis',(0.,0.,1.));
#16186=DIRECTION('refdir',(1.,0.,0.));
#16187=DIRECTION('',(0.342997170285005,0.939336436627729,0.));
#16188=DIRECTION('',(-0.342997170285022,-6.70692126230321E-16,-0.939336436627723));
#16189=DIRECTION('',(0.737980838656825,0.568079932640029,0.364238207643117));
#16190=DIRECTION('center_axis',(-1.,0.,0.));
#16191=DIRECTION('ref_axis',(0.,-1.,0.));
#16192=DIRECTION('',(0.707106781186544,0.352766841475276,0.612825877028347));
#16193=DIRECTION('center_axis',(-1.,0.,0.));
#16194=DIRECTION('ref_axis',(0.,-1.,0.));
#16195=DIRECTION('',(-0.707106781186552,-0.612825877028345,-0.352766841475263));
#16196=DIRECTION('center_axis',(1.,0.,0.));
#16197=DIRECTION('ref_axis',(0.,-1.,0.));
#16198=DIRECTION('',(-0.737980838656826,-0.364238207643135,-0.568079932640015));
#16199=DIRECTION('center_axis',(0.,1.,0.));
#16200=DIRECTION('ref_axis',(0.70710678118654,0.,-0.707106781186555));
#16201=DIRECTION('',(0.,1.,0.));
#16202=DIRECTION('',(0.,-1.,0.));
#16203=DIRECTION('center_axis',(0.,0.,-1.));
#16204=DIRECTION('ref_axis',(0.,-1.,0.));
#16205=DIRECTION('',(-1.,0.,0.));
#16206=DIRECTION('',(0.342997170284996,-0.939336436627732,0.));
#16207=DIRECTION('',(0.,-1.,0.));
#16208=DIRECTION('',(-1.,0.,0.));
#16209=DIRECTION('center_axis',(-1.,0.,0.));
#16210=DIRECTION('ref_axis',(0.,-1.,0.));
#16211=DIRECTION('',(-1.,0.,0.));
#16212=DIRECTION('center_axis',(-1.,0.,0.));
#16213=DIRECTION('ref_axis',(0.,-1.,0.));
#16214=DIRECTION('',(0.342997170285042,-2.68276850492132E-15,-0.939336436627715));
#16215=DIRECTION('',(-0.342997170285017,-0.939336436627724,0.));
#16216=DIRECTION('',(0.737980838656834,0.364238207643121,-0.568079932640014));
#16217=DIRECTION('center_axis',(-1.,0.,0.));
#16218=DIRECTION('ref_axis',(0.,-1.29526019539602E-15,1.));
#16219=DIRECTION('',(0.707106781186544,0.612825877028338,-0.352766841475291));
#16220=DIRECTION('center_axis',(-1.,0.,0.));
#16221=DIRECTION('ref_axis',(0.,-1.29526019539601E-15,1.));
#16222=DIRECTION('',(-0.707106781186543,-0.352766841475279,0.612825877028346));
#16223=DIRECTION('center_axis',(1.,0.,0.));
#16224=DIRECTION('ref_axis',(0.,-1.29526019539602E-15,1.));
#16225=DIRECTION('',(-0.737980838656842,-0.568079932640019,0.364238207643096));
#16226=DIRECTION('center_axis',(0.,0.,1.));
#16227=DIRECTION('ref_axis',(0.,1.,0.));
#16228=DIRECTION('',(0.,-1.,0.));
#16229=DIRECTION('',(-1.,0.,0.));
#16230=DIRECTION('',(0.,1.,0.));
#16231=DIRECTION('',(-0.342997170285038,0.939336436627717,0.));
#16232=DIRECTION('',(-1.,0.,0.));
#16233=DIRECTION('center_axis',(0.,-1.,0.));
#16234=DIRECTION('ref_axis',(0.707106781186548,0.,0.707106781186548));
#16235=DIRECTION('',(0.,1.,0.));
#16236=DIRECTION('center_axis',(1.,0.,0.));
#16237=DIRECTION('ref_axis',(0.,0.,-1.));
#16238=DIRECTION('center_axis',(1.,0.,0.));
#16239=DIRECTION('ref_axis',(0.,-2.96059473233375E-15,-1.));
#16240=DIRECTION('',(0.,0.,-1.));
#16241=DIRECTION('center_axis',(1.,0.,0.));
#16242=DIRECTION('ref_axis',(0.,1.,-3.7007434154172E-15));
#16243=DIRECTION('',(0.,0.,1.));
#16244=DIRECTION('',(-0.342997170285022,6.70692126230321E-16,0.939336436627723));
#16245=DIRECTION('',(-0.737980838656832,0.364238207643115,0.56807993264002));
#16246=DIRECTION('center_axis',(1.,0.,0.));
#16247=DIRECTION('ref_axis',(0.,-1.,0.));
#16248=DIRECTION('',(-0.707106781186552,0.612825877028345,0.352766841475263));
#16249=DIRECTION('center_axis',(1.,0.,0.));
#16250=DIRECTION('ref_axis',(0.,-1.,0.));
#16251=DIRECTION('',(0.707106781186544,-0.352766841475276,-0.612825877028347));
#16252=DIRECTION('',(0.737980838656822,-0.568079932640023,-0.364238207643131));
#16253=DIRECTION('center_axis',(0.,0.,1.));
#16254=DIRECTION('ref_axis',(-0.707106781186548,-0.707106781186548,0.));
#16255=DIRECTION('',(0.,0.,1.));
#16256=DIRECTION('',(0.,0.,-1.));
#16257=DIRECTION('center_axis',(0.,-1.,0.));
#16258=DIRECTION('ref_axis',(0.,0.,1.));
#16259=DIRECTION('',(0.,0.,-1.));
#16260=DIRECTION('',(-1.,0.,0.));
#16261=DIRECTION('',(0.342997170285042,2.68276850492132E-15,0.939336436627715));
#16262=DIRECTION('',(-0.737980838656821,0.568079932640026,-0.36423820764313));
#16263=DIRECTION('center_axis',(1.,0.,0.));
#16264=DIRECTION('ref_axis',(0.,-1.29526019539602E-15,1.));
#16265=DIRECTION('',(-0.707106781186543,0.352766841475279,-0.612825877028346));
#16266=DIRECTION('center_axis',(1.,0.,0.));
#16267=DIRECTION('ref_axis',(0.,-1.29526019539601E-15,1.));
#16268=DIRECTION('',(0.707106781186544,-0.612825877028338,0.352766841475291));
#16269=DIRECTION('center_axis',(-1.,0.,0.));
#16270=DIRECTION('ref_axis',(0.,-1.29526019539602E-15,1.));
#16271=DIRECTION('',(0.737980838656848,-0.36423820764311,0.568079932640002));
#16272=DIRECTION('center_axis',(1.,0.,0.));
#16273=DIRECTION('ref_axis',(0.,0.,-1.));
#16274=DIRECTION('',(0.,-1.,0.));
#16275=DIRECTION('center_axis',(-1.,0.,0.));
#16276=DIRECTION('ref_axis',(0.,1.,-3.7007434154172E-15));
#16277=DIRECTION('',(0.,0.,1.));
#16278=DIRECTION('center_axis',(-1.,0.,0.));
#16279=DIRECTION('ref_axis',(0.,-2.96059473233375E-15,-1.));
#16280=DIRECTION('',(0.,1.,0.));
#16281=DIRECTION('center_axis',(-1.,0.,0.));
#16282=DIRECTION('ref_axis',(0.,-1.29526019539602E-15,1.));
#16283=DIRECTION('center_axis',(0.,0.,-1.));
#16284=DIRECTION('ref_axis',(0.707106781186548,-0.707106781186548,0.));
#16285=DIRECTION('center_axis',(0.,1.,0.));
#16286=DIRECTION('ref_axis',(-0.707106781186548,0.,0.707106781186548));
#16287=DIRECTION('center_axis',(-1.,0.,0.));
#16288=DIRECTION('ref_axis',(0.,1.,-3.7007434154172E-15));
#16289=DIRECTION('',(-1.,0.,0.));
#16290=DIRECTION('center_axis',(0.,0.,-1.));
#16291=DIRECTION('ref_axis',(-0.70710678118654,0.707106781186555,0.));
#16292=DIRECTION('',(0.,0.,-1.));
#16293=DIRECTION('center_axis',(-1.,0.,0.));
#16294=DIRECTION('ref_axis',(0.,-2.96059473233375E-15,-1.));
#16295=DIRECTION('',(-1.,0.,0.));
#16296=DIRECTION('center_axis',(0.,1.,0.));
#16297=DIRECTION('ref_axis',(0.,0.,-1.));
#16298=DIRECTION('',(0.,0.,1.));
#16299=DIRECTION('center_axis',(0.,0.,1.));
#16300=DIRECTION('ref_axis',(0.70710678118654,0.707106781186555,0.));
#16301=DIRECTION('center_axis',(0.,-1.,0.));
#16302=DIRECTION('ref_axis',(-0.70710678118654,0.,-0.707106781186555));
#16303=DIRECTION('axis',(0.,0.,1.));
#16304=DIRECTION('refdir',(1.,0.,0.));
#16305=DIRECTION('',(0.707106781186503,0.,0.707106781186592));
#16306=DIRECTION('',(-0.707106781186503,0.,-0.707106781186592));
#16307=DIRECTION('',(0.707106781186563,0.,0.707106781186532));
#16308=DIRECTION('center_axis',(-0.707106781186548,0.,0.707106781186548));
#16309=DIRECTION('ref_axis',(0.707106781186548,0.,0.707106781186548));
#16310=DIRECTION('',(0.,-1.,0.));
#16311=DIRECTION('',(0.707106781186563,0.,0.707106781186532));
#16312=DIRECTION('',(0.,1.,0.));
#16313=DIRECTION('center_axis',(0.,1.,0.));
#16314=DIRECTION('ref_axis',(1.,0.,0.));
#16315=DIRECTION('',(0.,0.,1.));
#16316=DIRECTION('',(-0.70710678118657,0.,0.707106781186525));
#16317=DIRECTION('',(-1.,0.,0.));
#16318=DIRECTION('',(-0.707106781186556,0.,-0.707106781186539));
#16319=DIRECTION('',(0.,0.,-1.));
#16320=DIRECTION('',(0.707106781186545,0.,-0.70710678118655));
#16321=DIRECTION('',(1.,0.,0.));
#16322=DIRECTION('center_axis',(0.,0.,-1.));
#16323=DIRECTION('ref_axis',(-0.707106781186555,-0.70710678118654,0.));
#16324=DIRECTION('',(0.,0.,-1.));
#16325=DIRECTION('center_axis',(-1.,0.,0.));
#16326=DIRECTION('ref_axis',(0.,0.,1.));
#16327=DIRECTION('',(0.,0.,1.));
#16328=DIRECTION('',(0.,1.,0.));
#16329=DIRECTION('center_axis',(0.,0.,1.));
#16330=DIRECTION('ref_axis',(-0.707106781186555,0.70710678118654,0.));
#16331=DIRECTION('',(0.,0.,-1.));
#16332=DIRECTION('',(0.70710678118657,0.,-0.707106781186525));
#16333=DIRECTION('',(0.707106781186548,0.,-0.707106781186548));
#16334=DIRECTION('center_axis',(-0.707106781186548,0.,-0.707106781186548));
#16335=DIRECTION('ref_axis',(-0.707106781186548,0.,0.707106781186548));
#16336=DIRECTION('',(0.707106781186548,0.,-0.707106781186548));
#16337=DIRECTION('',(0.,-1.,0.));
#16338=DIRECTION('',(0.707106781186511,0.,0.707106781186584));
#16339=DIRECTION('',(-0.707106781186563,0.,-0.707106781186532));
#16340=DIRECTION('center_axis',(0.707106781186538,0.,-0.707106781186557));
#16341=DIRECTION('ref_axis',(-0.707106781186557,0.,-0.707106781186538));
#16342=DIRECTION('',(0.,-1.,0.));
#16343=DIRECTION('',(-0.707106781186557,0.,-0.707106781186538));
#16344=DIRECTION('',(0.,1.,0.));
#16345=DIRECTION('center_axis',(0.,0.,1.));
#16346=DIRECTION('ref_axis',(0.707106781186555,-0.70710678118654,0.));
#16347=DIRECTION('',(0.,0.,1.));
#16348=DIRECTION('center_axis',(1.,0.,0.));
#16349=DIRECTION('ref_axis',(0.,0.,-1.));
#16350=DIRECTION('',(0.,0.,-1.));
#16351=DIRECTION('',(0.,1.,0.));
#16352=DIRECTION('center_axis',(0.,0.,-1.));
#16353=DIRECTION('ref_axis',(0.707106781186555,0.70710678118654,0.));
#16354=DIRECTION('',(0.,0.,1.));
#16355=DIRECTION('center_axis',(0.,1.,0.));
#16356=DIRECTION('ref_axis',(0.,0.,1.));
#16357=DIRECTION('',(-1.,0.,0.));
#16358=DIRECTION('',(-0.707106781186534,0.,0.707106781186561));
#16359=DIRECTION('',(1.,0.,0.));
#16360=DIRECTION('',(0.707106781186575,0.,-0.70710678118652));
#16361=DIRECTION('center_axis',(0.707106781186538,0.,0.707106781186557));
#16362=DIRECTION('ref_axis',(0.707106781186557,0.,-0.707106781186538));
#16363=DIRECTION('',(0.,-1.,0.));
#16364=DIRECTION('',(0.707106781186557,0.,-0.707106781186538));
#16365=DIRECTION('center_axis',(-1.,0.,0.));
#16366=DIRECTION('ref_axis',(0.,-0.70710678118654,0.707106781186555));
#16367=DIRECTION('',(-1.,0.,0.));
#16368=DIRECTION('center_axis',(0.,0.,1.));
#16369=DIRECTION('ref_axis',(1.,0.,0.));
#16370=DIRECTION('',(1.,0.,0.));
#16371=DIRECTION('center_axis',(1.,0.,0.));
#16372=DIRECTION('ref_axis',(0.,0.70710678118654,0.707106781186555));
#16373=DIRECTION('center_axis',(-1.,0.,0.));
#16374=DIRECTION('ref_axis',(0.,0.707106781186532,-0.707106781186563));
#16375=DIRECTION('',(-1.,0.,0.));
#16376=DIRECTION('center_axis',(0.,0.,-1.));
#16377=DIRECTION('ref_axis',(-1.,0.,0.));
#16378=DIRECTION('',(1.,0.,0.));
#16379=DIRECTION('center_axis',(1.,0.,0.));
#16380=DIRECTION('ref_axis',(0.,-0.707106781186532,-0.707106781186563));
#16381=DIRECTION('axis',(0.,0.,1.));
#16382=DIRECTION('refdir',(1.,0.,0.));
#16383=DIRECTION('center_axis',(0.,-1.,0.));
#16384=DIRECTION('ref_axis',(-4.93432455388959E-16,0.,1.));
#16385=DIRECTION('center_axis',(0.,1.,0.));
#16386=DIRECTION('ref_axis',(-4.93432455388959E-16,0.,1.));
#16387=DIRECTION('',(-0.707106781186548,0.707106781186548,0.));
#16388=DIRECTION('center_axis',(0.,-1.,0.));
#16389=DIRECTION('ref_axis',(-4.93432455388959E-16,0.,1.));
#16390=DIRECTION('center_axis',(0.707106781186548,0.707106781186548,0.));
#16391=DIRECTION('ref_axis',(0.,0.,-1.));
#16392=DIRECTION('',(0.,0.,-1.));
#16393=DIRECTION('',(-0.707106781186548,0.707106781186548,0.));
#16394=DIRECTION('',(0.,0.,1.));
#16395=DIRECTION('center_axis',(0.,-1.,0.));
#16396=DIRECTION('ref_axis',(1.,0.,2.46716227694479E-16));
#16397=DIRECTION('center_axis',(0.,-1.,0.));
#16398=DIRECTION('ref_axis',(1.,0.,2.46716227694479E-16));
#16399=DIRECTION('center_axis',(0.,1.,0.));
#16400=DIRECTION('ref_axis',(1.,0.,2.46716227694479E-16));
#16401=DIRECTION('center_axis',(0.,-1.,0.));
#16402=DIRECTION('ref_axis',(1.,0.,2.46716227694479E-16));
#16403=DIRECTION('',(0.,-1.,0.));
#16404=DIRECTION('',(0.,-1.,0.));
#16405=DIRECTION('center_axis',(0.,-1.,0.));
#16406=DIRECTION('ref_axis',(1.,0.,2.46716227694479E-16));
#16407=DIRECTION('',(0.,-1.,0.));
#16408=DIRECTION('center_axis',(0.,1.,0.));
#16409=DIRECTION('ref_axis',(1.,0.,2.46716227694479E-16));
#16410=DIRECTION('center_axis',(0.707106781186548,-0.707106781186548,0.));
#16411=DIRECTION('ref_axis',(0.707106781186547,0.707106781186547,1.74454717631531E-16));
#16412=DIRECTION('center_axis',(1.,0.,0.));
#16413=DIRECTION('ref_axis',(0.,0.,1.));
#16414=DIRECTION('',(0.,-1.,0.));
#16415=DIRECTION('',(0.,0.,1.));
#16416=DIRECTION('center_axis',(-1.,0.,0.));
#16417=DIRECTION('ref_axis',(0.,0.,-1.));
#16418=DIRECTION('center_axis',(0.,-1.,0.));
#16419=DIRECTION('ref_axis',(-4.93432455388959E-16,0.,1.));
#16420=DIRECTION('',(0.,1.,0.));
#16421=DIRECTION('center_axis',(0.707106781186548,-0.707106781186548,0.));
#16422=DIRECTION('ref_axis',(-0.707106781186547,-0.707106781186547,-3.48909435263061E-16));
#16423=DIRECTION('center_axis',(0.,1.,0.));
#16424=DIRECTION('ref_axis',(-4.93432455388959E-16,0.,1.));
#16425=DIRECTION('',(0.,-1.,0.));
#16426=DIRECTION('center_axis',(0.,-1.,0.));
#16427=DIRECTION('ref_axis',(-4.93432455388959E-16,0.,1.));
#16428=DIRECTION('center_axis',(0.,1.,0.));
#16429=DIRECTION('ref_axis',(1.,0.,0.));
#16430=DIRECTION('center_axis',(0.,1.,0.));
#16431=DIRECTION('ref_axis',(1.,0.,0.));
#16432=DIRECTION('',(0.707106781186546,-0.707106781186549,-8.65956056235492E-17));
#16433=DIRECTION('center_axis',(0.,-1.,0.));
#16434=DIRECTION('ref_axis',(1.,0.,0.));
#16435=DIRECTION('center_axis',(0.,1.,0.));
#16436=DIRECTION('ref_axis',(1.,0.,0.));
#16437=DIRECTION('center_axis',(0.,-1.,0.));
#16438=DIRECTION('ref_axis',(2.22044604925031E-15,0.,1.));
#16439=DIRECTION('',(0.,0.,1.));
#16440=DIRECTION('center_axis',(0.,-1.,0.));
#16441=DIRECTION('ref_axis',(1.,0.,0.));
#16442=DIRECTION('',(1.,0.,0.));
#16443=DIRECTION('center_axis',(0.,-1.,0.));
#16444=DIRECTION('ref_axis',(-4.16333634234433E-16,0.,-1.));
#16445=DIRECTION('',(0.,0.,-1.));
#16446=DIRECTION('center_axis',(0.,-1.,0.));
#16447=DIRECTION('ref_axis',(-1.,0.,1.11022302462516E-15));
#16448=DIRECTION('',(-1.,0.,0.));
#16449=DIRECTION('center_axis',(0.,-1.,0.));
#16450=DIRECTION('ref_axis',(1.,0.,0.));
#16451=DIRECTION('',(0.,-1.,0.));
#16452=DIRECTION('center_axis',(0.,-1.,0.));
#16453=DIRECTION('ref_axis',(1.,0.,0.));
#16454=DIRECTION('center_axis',(0.,-1.,0.));
#16455=DIRECTION('ref_axis',(-1.85037170770859E-16,0.,-1.));
#16456=DIRECTION('center_axis',(0.,1.,0.));
#16457=DIRECTION('ref_axis',(-1.85037170770859E-16,0.,-1.));
#16458=DIRECTION('',(0.707106781186548,0.707106781186547,7.85046229341889E-16));
#16459=DIRECTION('center_axis',(0.,-1.,0.));
#16460=DIRECTION('ref_axis',(-1.85037170770859E-16,0.,-1.));
#16461=DIRECTION('center_axis',(-0.707106781186545,0.70710678118655,0.));
#16462=DIRECTION('ref_axis',(0.,0.,1.));
#16463=DIRECTION('',(0.,0.,1.));
#16464=DIRECTION('',(0.70710678118655,0.707106781186545,0.));
#16465=DIRECTION('',(0.,0.,-1.));
#16466=DIRECTION('center_axis',(0.,-1.,0.));
#16467=DIRECTION('ref_axis',(-1.,0.,0.));
#16468=DIRECTION('center_axis',(0.,-1.,0.));
#16469=DIRECTION('ref_axis',(-1.,0.,0.));
#16470=DIRECTION('center_axis',(0.,1.,0.));
#16471=DIRECTION('ref_axis',(-1.,0.,0.));
#16472=DIRECTION('center_axis',(0.,-1.,0.));
#16473=DIRECTION('ref_axis',(-1.,0.,0.));
#16474=DIRECTION('',(0.,-1.,0.));
#16475=DIRECTION('',(0.,-1.,0.));
#16476=DIRECTION('center_axis',(0.,-1.,0.));
#16477=DIRECTION('ref_axis',(-1.,0.,0.));
#16478=DIRECTION('',(0.,-1.,0.));
#16479=DIRECTION('center_axis',(0.,1.,0.));
#16480=DIRECTION('ref_axis',(-1.,0.,0.));
#16481=DIRECTION('center_axis',(-0.707106781186546,-0.707106781186549,0.));
#16482=DIRECTION('ref_axis',(-0.707106781186549,0.707106781186546,0.));
#16483=DIRECTION('center_axis',(-1.,0.,0.));
#16484=DIRECTION('ref_axis',(0.,0.,-1.));
#16485=DIRECTION('',(0.,-1.,0.));
#16486=DIRECTION('',(0.,0.,-1.));
#16487=DIRECTION('center_axis',(1.,0.,0.));
#16488=DIRECTION('ref_axis',(0.,0.,-1.));
#16489=DIRECTION('center_axis',(0.,-1.,0.));
#16490=DIRECTION('ref_axis',(-1.85037170770859E-16,0.,-1.));
#16491=DIRECTION('',(0.,1.,0.));
#16492=DIRECTION('center_axis',(-0.707106781186546,-0.707106781186549,0.));
#16493=DIRECTION('ref_axis',(0.707106781186549,-0.707106781186546,-1.30841038223648E-16));
#16494=DIRECTION('center_axis',(0.,1.,0.));
#16495=DIRECTION('ref_axis',(-1.85037170770859E-16,0.,-1.));
#16496=DIRECTION('',(0.,-1.,0.));
#16497=DIRECTION('center_axis',(0.,-1.,0.));
#16498=DIRECTION('ref_axis',(-1.85037170770859E-16,0.,-1.));
#16499=DIRECTION('center_axis',(-0.707106781186546,-0.707106781186549,0.));
#16500=DIRECTION('ref_axis',(0.,0.,1.));
#16501=DIRECTION('',(0.,0.,-1.));
#16502=DIRECTION('',(0.707106781186549,-0.707106781186546,0.));
#16503=DIRECTION('',(0.,0.,1.));
#16504=DIRECTION('center_axis',(0.,1.,0.));
#16505=DIRECTION('ref_axis',(-4.16333634234433E-16,0.,-1.));
#16506=DIRECTION('',(3.92523114670945E-16,-0.707106781186548,0.707106781186548));
#16507=DIRECTION('center_axis',(0.,1.,0.));
#16508=DIRECTION('ref_axis',(-4.16333634234433E-16,0.,-1.));
#16509=DIRECTION('center_axis',(0.,-1.,0.));
#16510=DIRECTION('ref_axis',(-4.16333634234433E-16,0.,-1.));
#16511=DIRECTION('center_axis',(0.,-0.707106781186549,-0.707106781186546));
#16512=DIRECTION('ref_axis',(-1.,0.,0.));
#16513=DIRECTION('',(0.,-0.707106781186544,0.707106781186551));
#16514=DIRECTION('',(-1.,0.,0.));
#16515=DIRECTION('',(1.,0.,0.));
#16516=DIRECTION('center_axis',(0.,1.,0.));
#16517=DIRECTION('ref_axis',(1.,0.,0.));
#16518=DIRECTION('',(-0.707106781186548,-0.707106781186548,0.));
#16519=DIRECTION('center_axis',(0.,1.,0.));
#16520=DIRECTION('ref_axis',(1.,0.,0.));
#16521=DIRECTION('center_axis',(0.,-1.,0.));
#16522=DIRECTION('ref_axis',(1.,0.,0.));
#16523=DIRECTION('center_axis',(0.707106781186548,-0.707106781186548,0.));
#16524=DIRECTION('ref_axis',(0.,0.,-1.));
#16525=DIRECTION('',(0.,0.,-1.));
#16526=DIRECTION('',(0.,0.,1.));
#16527=DIRECTION('center_axis',(1.,0.,0.));
#16528=DIRECTION('ref_axis',(0.,0.,1.));
#16529=DIRECTION('',(0.,-1.,0.));
#16530=DIRECTION('',(0.,0.,-1.));
#16531=DIRECTION('',(0.,-1.,0.));
#16532=DIRECTION('',(0.,0.,1.));
#16533=DIRECTION('',(0.,1.,0.));
#16534=DIRECTION('',(0.,0.,-1.));
#16535=DIRECTION('',(0.,-1.,0.));
#16536=DIRECTION('',(0.,0.,1.));
#16537=DIRECTION('',(0.,0.,1.));
#16538=DIRECTION('center_axis',(0.,-1.,0.));
#16539=DIRECTION('ref_axis',(1.,0.,0.));
#16540=DIRECTION('',(0.,-1.,0.));
#16541=DIRECTION('center_axis',(0.,1.,0.));
#16542=DIRECTION('ref_axis',(1.,0.,0.));
#16543=DIRECTION('center_axis',(0.,0.,-1.));
#16544=DIRECTION('ref_axis',(1.,0.,0.));
#16545=DIRECTION('',(0.,-1.,0.));
#16546=DIRECTION('',(-1.,0.,0.));
#16547=DIRECTION('center_axis',(0.,-1.,0.));
#16548=DIRECTION('ref_axis',(-4.16333634234433E-16,0.,-1.));
#16549=DIRECTION('',(0.,-1.,0.));
#16550=DIRECTION('center_axis',(0.,1.,0.));
#16551=DIRECTION('ref_axis',(-4.16333634234433E-16,0.,-1.));
#16552=DIRECTION('center_axis',(-1.,0.,0.));
#16553=DIRECTION('ref_axis',(0.,0.,-1.));
#16554=DIRECTION('',(0.,0.,-1.));
#16555=DIRECTION('',(0.,0.,-1.));
#16556=DIRECTION('',(0.,-1.,0.));
#16557=DIRECTION('',(0.,0.,1.));
#16558=DIRECTION('',(0.,-1.,0.));
#16559=DIRECTION('',(0.,0.,-1.));
#16560=DIRECTION('',(0.,-1.,0.));
#16561=DIRECTION('',(0.,0.,1.));
#16562=DIRECTION('center_axis',(0.707106781186548,-0.707106781186548,0.));
#16563=DIRECTION('ref_axis',(0.,0.,-1.));
#16564=DIRECTION('',(-0.707106781186544,-0.707106781186551,0.));
#16565=DIRECTION('',(0.,0.,-1.));
#16566=DIRECTION('center_axis',(0.,1.,0.));
#16567=DIRECTION('ref_axis',(2.22044604925031E-15,0.,1.));
#16568=DIRECTION('',(0.,-0.707106781186548,-0.707106781186548));
#16569=DIRECTION('center_axis',(0.,1.,0.));
#16570=DIRECTION('ref_axis',(2.22044604925031E-15,0.,1.));
#16571=DIRECTION('center_axis',(0.,-1.,0.));
#16572=DIRECTION('ref_axis',(2.22044604925031E-15,0.,1.));
#16573=DIRECTION('center_axis',(0.,-0.707106781186549,0.707106781186546));
#16574=DIRECTION('ref_axis',(1.,0.,0.));
#16575=DIRECTION('',(0.,-0.707106781186546,-0.707106781186549));
#16576=DIRECTION('',(1.,0.,0.));
#16577=DIRECTION('',(-1.,0.,0.));
#16578=DIRECTION('center_axis',(0.,1.,0.));
#16579=DIRECTION('ref_axis',(-1.,0.,1.11022302462516E-15));
#16580=DIRECTION('',(0.707106781186548,-0.707106781186547,0.));
#16581=DIRECTION('center_axis',(0.,1.,0.));
#16582=DIRECTION('ref_axis',(-1.,0.,1.11022302462516E-15));
#16583=DIRECTION('center_axis',(0.,-1.,0.));
#16584=DIRECTION('ref_axis',(-1.,0.,1.11022302462516E-15));
#16585=DIRECTION('center_axis',(-0.707106781186546,-0.707106781186549,0.));
#16586=DIRECTION('ref_axis',(0.,0.,1.));
#16587=DIRECTION('',(0.,0.,1.));
#16588=DIRECTION('center_axis',(0.,-1.,0.));
#16589=DIRECTION('ref_axis',(-1.,0.,1.11022302462516E-15));
#16590=DIRECTION('',(0.,-1.,0.));
#16591=DIRECTION('center_axis',(0.,1.,0.));
#16592=DIRECTION('ref_axis',(-1.,0.,1.11022302462516E-15));
#16593=DIRECTION('center_axis',(0.,0.,1.));
#16594=DIRECTION('ref_axis',(-1.,0.,0.));
#16595=DIRECTION('',(0.,-1.,0.));
#16596=DIRECTION('',(1.,0.,0.));
#16597=DIRECTION('center_axis',(0.,-1.,0.));
#16598=DIRECTION('ref_axis',(2.22044604925031E-15,0.,1.));
#16599=DIRECTION('center_axis',(0.,1.,0.));
#16600=DIRECTION('ref_axis',(2.22044604925031E-15,0.,1.));
#16601=DIRECTION('center_axis',(0.,-1.,0.));
#16602=DIRECTION('ref_axis',(2.22044604925031E-15,0.,1.));
#16603=DIRECTION('',(-0.707106781186546,0.707106781186549,0.));
#16604=DIRECTION('',(0.,-0.707106781186549,0.707106781186546));
#16605=DIRECTION('center_axis',(0.,1.,0.));
#16606=DIRECTION('ref_axis',(2.22044604925031E-15,0.,1.));
#16607=DIRECTION('center_axis',(0.707106781186549,0.707106781186546,0.));
#16608=DIRECTION('ref_axis',(0.,0.,-1.));
#16609=DIRECTION('',(-0.707106781186546,0.707106781186549,0.));
#16610=DIRECTION('center_axis',(0.,-1.,0.));
#16611=DIRECTION('ref_axis',(1.,0.,0.));
#16612=DIRECTION('',(0.,0.707106781186549,0.707106781186546));
#16613=DIRECTION('center_axis',(0.,0.707106781186548,-0.707106781186547));
#16614=DIRECTION('ref_axis',(-1.,0.,0.));
#16615=DIRECTION('',(0.,0.707106781186547,0.707106781186548));
#16616=DIRECTION('center_axis',(0.,-1.,0.));
#16617=DIRECTION('ref_axis',(-4.16333634234433E-16,0.,-1.));
#16618=DIRECTION('',(0.707106781186547,0.707106781186548,0.));
#16619=DIRECTION('center_axis',(-0.707106781186548,0.707106781186547,0.));
#16620=DIRECTION('ref_axis',(0.,0.,1.));
#16621=DIRECTION('',(0.707106781186547,0.707106781186548,0.));
#16622=DIRECTION('center_axis',(0.,-1.,0.));
#16623=DIRECTION('ref_axis',(-1.,0.,1.11022302462516E-15));
#16624=DIRECTION('',(3.92523114670944E-16,0.707106781186547,-0.707106781186548));
#16625=DIRECTION('center_axis',(0.,1.,0.));
#16626=DIRECTION('ref_axis',(-1.,0.,1.11022302462516E-15));
#16627=DIRECTION('center_axis',(0.,0.707106781186548,0.707106781186547));
#16628=DIRECTION('ref_axis',(1.,0.,0.));
#16629=DIRECTION('',(1.,0.,0.));
#16630=DIRECTION('center_axis',(0.,-1.,0.));
#16631=DIRECTION('ref_axis',(2.22044604925031E-15,0.,1.));
#16632=DIRECTION('',(0.,-1.,0.));
#16633=DIRECTION('center_axis',(0.,-1.,0.));
#16634=DIRECTION('ref_axis',(2.22044604925031E-15,0.,1.));
#16635=DIRECTION('center_axis',(-0.707106781186549,0.,0.707106781186546));
#16636=DIRECTION('ref_axis',(0.707106781186546,0.,0.707106781186549));
#16637=DIRECTION('',(-0.577350269189625,-0.577350269189625,-0.577350269189627));
#16638=DIRECTION('',(0.,1.,0.));
#16639=DIRECTION('',(0.577350269189625,-0.577350269189626,0.577350269189627));
#16640=DIRECTION('center_axis',(0.,0.,-1.));
#16641=DIRECTION('ref_axis',(-1.,0.,0.));
#16642=DIRECTION('',(-1.,0.,0.));
#16643=DIRECTION('',(0.,-1.,0.));
#16644=DIRECTION('',(1.,0.,0.));
#16645=DIRECTION('center_axis',(0.707106781186554,0.,0.707106781186541));
#16646=DIRECTION('ref_axis',(0.707106781186541,0.,-0.707106781186554));
#16647=DIRECTION('',(0.577350269189622,0.577350269189624,-0.577350269189632));
#16648=DIRECTION('',(-0.577350269189622,0.577350269189624,0.577350269189632));
#16649=DIRECTION('center_axis',(0.,1.,0.));
#16650=DIRECTION('ref_axis',(1.,0.,2.46716227694479E-16));
#16651=DIRECTION('',(-0.707106781186548,-0.707106781186548,0.));
#16652=DIRECTION('center_axis',(0.,1.,0.));
#16653=DIRECTION('ref_axis',(1.,0.,2.46716227694479E-16));
#16654=DIRECTION('',(6.28036983473511E-15,0.707106781186546,-0.707106781186549));
#16655=DIRECTION('center_axis',(0.707106781186548,-0.707106781186548,0.));
#16656=DIRECTION('ref_axis',(0.,0.,-1.));
#16657=DIRECTION('',(-0.707106781186551,-0.707106781186544,7.85046229341887E-16));
#16658=DIRECTION('',(0.,0.,-1.));
#16659=DIRECTION('center_axis',(0.,1.,0.));
#16660=DIRECTION('ref_axis',(-4.93432455388959E-16,0.,1.));
#16661=DIRECTION('',(0.,-0.707106781186546,-0.707106781186549));
#16662=DIRECTION('center_axis',(0.,1.,0.));
#16663=DIRECTION('ref_axis',(-4.93432455388959E-16,0.,1.));
#16664=DIRECTION('center_axis',(0.,-0.707106781186549,0.707106781186546));
#16665=DIRECTION('ref_axis',(1.,0.,0.));
#16666=DIRECTION('',(7.85046229341889E-16,-0.707106781186546,-0.707106781186549));
#16667=DIRECTION('',(1.,0.,0.));
#16668=DIRECTION('',(-1.,0.,0.));
#16669=DIRECTION('center_axis',(0.,1.,0.));
#16670=DIRECTION('ref_axis',(-1.,0.,0.));
#16671=DIRECTION('',(0.707106781186548,-0.707106781186547,0.));
#16672=DIRECTION('center_axis',(0.,1.,0.));
#16673=DIRECTION('ref_axis',(-1.,0.,0.));
#16674=DIRECTION('center_axis',(-0.707106781186545,-0.70710678118655,0.));
#16675=DIRECTION('ref_axis',(0.,0.,1.));
#16676=DIRECTION('',(0.70710678118655,-0.707106781186545,-7.85046229341888E-16));
#16677=DIRECTION('',(0.,0.,1.));
#16678=DIRECTION('center_axis',(0.,1.,0.));
#16679=DIRECTION('ref_axis',(-1.85037170770859E-16,0.,-1.));
#16680=DIRECTION('',(0.,-0.707106781186546,0.707106781186549));
#16681=DIRECTION('center_axis',(0.,1.,0.));
#16682=DIRECTION('ref_axis',(-1.85037170770859E-16,0.,-1.));
#16683=DIRECTION('center_axis',(0.,-0.707106781186549,-0.707106781186546));
#16684=DIRECTION('ref_axis',(-1.,0.,0.));
#16685=DIRECTION('',(-1.,0.,0.));
#16686=DIRECTION('',(1.,0.,0.));
#16687=DIRECTION('center_axis',(0.,0.,1.));
#16688=DIRECTION('ref_axis',(-1.,0.,0.));
#16689=DIRECTION('',(1.,0.,0.));
#16690=DIRECTION('center_axis',(0.,1.,0.));
#16691=DIRECTION('ref_axis',(1.,0.,0.));
#16692=DIRECTION('',(0.,0.,-1.));
#16693=DIRECTION('',(-1.,0.,0.));
#16694=DIRECTION('',(0.,0.,1.));
#16695=DIRECTION('',(1.,0.,0.));
#16696=DIRECTION('',(0.,0.,-1.));
#16697=DIRECTION('',(-1.,0.,0.));
#16698=DIRECTION('',(0.,0.,1.));
#16699=DIRECTION('',(1.,0.,0.));
#16700=DIRECTION('',(0.,0.,-1.));
#16701=DIRECTION('',(-1.,0.,0.));
#16702=DIRECTION('',(0.,0.,1.));
#16703=DIRECTION('',(1.,0.,0.));
#16704=DIRECTION('',(0.,0.,-1.));
#16705=DIRECTION('',(-1.,0.,0.));
#16706=DIRECTION('',(0.,0.,1.));
#16707=DIRECTION('',(1.,0.,0.));
#16708=DIRECTION('center_axis',(-0.707106781186548,-0.707106781186547,0.));
#16709=DIRECTION('ref_axis',(0.,0.,1.));
#16710=DIRECTION('',(0.,0.,1.));
#16711=DIRECTION('',(-0.707106781186547,0.707106781186548,0.));
#16712=DIRECTION('center_axis',(0.,1.,0.));
#16713=DIRECTION('ref_axis',(-1.,0.,1.11022302462516E-15));
#16714=DIRECTION('',(-3.92523114670943E-16,0.707106781186547,0.707106781186547));
#16715=DIRECTION('center_axis',(0.,-1.,0.));
#16716=DIRECTION('ref_axis',(-1.,0.,1.11022302462516E-15));
#16717=DIRECTION('center_axis',(0.,1.,0.));
#16718=DIRECTION('ref_axis',(-1.,0.,1.11022302462516E-15));
#16719=DIRECTION('center_axis',(0.,-0.707106781186548,0.707106781186548));
#16720=DIRECTION('ref_axis',(1.,0.,0.));
#16721=DIRECTION('',(0.,0.707106781186547,0.707106781186547));
#16722=DIRECTION('',(-1.,0.,0.));
#16723=DIRECTION('',(1.,0.,0.));
#16724=DIRECTION('center_axis',(0.,1.,0.));
#16725=DIRECTION('ref_axis',(2.22044604925031E-15,0.,1.));
#16726=DIRECTION('',(0.707106781186546,0.707106781186549,0.));
#16727=DIRECTION('center_axis',(0.,1.,0.));
#16728=DIRECTION('ref_axis',(2.22044604925031E-15,0.,1.));
#16729=DIRECTION('center_axis',(0.707106781186549,-0.707106781186546,0.));
#16730=DIRECTION('ref_axis',(0.,0.,-1.));
#16731=DIRECTION('',(0.,0.,-1.));
#16732=DIRECTION('center_axis',(0.,1.,0.));
#16733=DIRECTION('ref_axis',(1.,0.,0.));
#16734=DIRECTION('center_axis',(0.707106781186549,0.707106781186546,0.));
#16735=DIRECTION('ref_axis',(0.,0.,-1.));
#16736=DIRECTION('',(0.,0.,1.));
#16737=DIRECTION('',(0.707106781186543,-0.707106781186552,0.));
#16738=DIRECTION('center_axis',(0.,-1.,0.));
#16739=DIRECTION('ref_axis',(2.22044604925031E-15,0.,1.));
#16740=DIRECTION('',(0.,-0.707106781186549,0.707106781186546));
#16741=DIRECTION('center_axis',(0.,-1.,0.));
#16742=DIRECTION('ref_axis',(2.22044604925031E-15,0.,1.));
#16743=DIRECTION('center_axis',(0.,0.707106781186548,0.707106781186548));
#16744=DIRECTION('ref_axis',(1.,0.,0.));
#16745=DIRECTION('',(0.,-0.707106781186547,0.707106781186547));
#16746=DIRECTION('',(-1.,0.,0.));
#16747=DIRECTION('center_axis',(0.,-1.,0.));
#16748=DIRECTION('ref_axis',(-1.,0.,1.11022302462516E-15));
#16749=DIRECTION('',(-0.707106781186546,-0.707106781186549,0.));
#16750=DIRECTION('center_axis',(0.,-1.,0.));
#16751=DIRECTION('ref_axis',(-1.,0.,1.11022302462516E-15));
#16752=DIRECTION('center_axis',(-0.707106781186547,0.707106781186548,0.));
#16753=DIRECTION('ref_axis',(0.,0.,1.));
#16754=DIRECTION('',(0.,0.,-1.));
#16755=DIRECTION('center_axis',(0.,-1.,0.));
#16756=DIRECTION('ref_axis',(-1.,0.,0.));
#16757=DIRECTION('center_axis',(-0.707106781186554,-0.707106781186541,0.));
#16758=DIRECTION('ref_axis',(0.,0.,1.));
#16759=DIRECTION('',(-0.577350269189622,0.577350269189632,-0.577350269189624));
#16760=DIRECTION('',(0.,0.,-1.));
#16761=DIRECTION('',(-0.577350269189622,0.577350269189632,0.577350269189623));
#16762=DIRECTION('center_axis',(0.707106781186554,-0.707106781186541,0.));
#16763=DIRECTION('ref_axis',(0.,0.,-1.));
#16764=DIRECTION('',(0.577350269189622,0.577350269189632,0.577350269189624));
#16765=DIRECTION('',(0.,0.,1.));
#16766=DIRECTION('',(-0.577350269189622,-0.577350269189632,0.577350269189624));
#16767=DIRECTION('center_axis',(0.,-0.707106781186543,0.707106781186552));
#16768=DIRECTION('ref_axis',(1.,0.,0.));
#16769=DIRECTION('',(-1.,0.,0.));
#16770=DIRECTION('center_axis',(0.,-0.707106781186543,-0.707106781186552));
#16771=DIRECTION('ref_axis',(-1.,0.,0.));
#16772=DIRECTION('',(1.,0.,0.));
#16773=DIRECTION('center_axis',(0.,0.,1.));
#16774=DIRECTION('ref_axis',(1.,0.,0.));
#16775=DIRECTION('',(0.,1.,0.));
#16776=DIRECTION('',(1.,0.,0.));
#16777=DIRECTION('',(0.,1.,0.));
#16778=DIRECTION('center_axis',(-1.,0.,0.));
#16779=DIRECTION('ref_axis',(0.,0.,1.));
#16780=DIRECTION('',(0.,1.,0.));
#16781=DIRECTION('',(0.,0.,1.));
#16782=DIRECTION('center_axis',(-1.,0.,0.));
#16783=DIRECTION('ref_axis',(0.,0.,-1.));
#16784=DIRECTION('center_axis',(-0.707106781186553,-0.707106781186542,0.));
#16785=DIRECTION('ref_axis',(0.,0.,1.));
#16786=DIRECTION('',(-0.577350269189623,0.577350269189631,-0.577350269189623));
#16787=DIRECTION('',(0.,0.,-1.));
#16788=DIRECTION('',(-0.577350269189623,0.577350269189632,0.577350269189623));
#16789=DIRECTION('center_axis',(0.707106781186553,-0.707106781186542,0.));
#16790=DIRECTION('ref_axis',(0.,0.,-1.));
#16791=DIRECTION('',(0.577350269189622,0.577350269189631,0.577350269189624));
#16792=DIRECTION('',(0.,0.,1.));
#16793=DIRECTION('',(-0.577350269189622,-0.577350269189631,0.577350269189624));
#16794=DIRECTION('center_axis',(0.,-0.707106781186543,0.707106781186552));
#16795=DIRECTION('ref_axis',(1.,0.,0.));
#16796=DIRECTION('',(-1.,0.,0.));
#16797=DIRECTION('center_axis',(0.,-0.707106781186543,-0.707106781186552));
#16798=DIRECTION('ref_axis',(-1.,0.,0.));
#16799=DIRECTION('',(1.,0.,0.));
#16800=DIRECTION('center_axis',(0.,0.,1.));
#16801=DIRECTION('ref_axis',(1.,0.,0.));
#16802=DIRECTION('',(0.,1.,0.));
#16803=DIRECTION('',(1.,0.,0.));
#16804=DIRECTION('',(0.,1.,0.));
#16805=DIRECTION('center_axis',(-1.,0.,0.));
#16806=DIRECTION('ref_axis',(0.,0.,1.));
#16807=DIRECTION('',(0.,1.,0.));
#16808=DIRECTION('',(0.,0.,1.));
#16809=DIRECTION('center_axis',(-1.,0.,0.));
#16810=DIRECTION('ref_axis',(0.,0.,-1.));
#16811=DIRECTION('center_axis',(-0.707106781186551,-0.707106781186544,0.));
#16812=DIRECTION('ref_axis',(0.,0.,1.));
#16813=DIRECTION('',(-0.577350269189625,0.57735026918963,-0.577350269189622));
#16814=DIRECTION('',(0.,0.,-1.));
#16815=DIRECTION('',(-0.577350269189625,0.577350269189631,0.577350269189622));
#16816=DIRECTION('center_axis',(0.707106781186552,-0.707106781186543,0.));
#16817=DIRECTION('ref_axis',(0.,0.,-1.));
#16818=DIRECTION('',(0.577350269189623,0.577350269189631,0.577350269189623));
#16819=DIRECTION('',(0.,0.,1.));
#16820=DIRECTION('',(-0.577350269189623,-0.577350269189631,0.577350269189623));
#16821=DIRECTION('center_axis',(0.,-0.707106781186543,0.707106781186552));
#16822=DIRECTION('ref_axis',(1.,0.,0.));
#16823=DIRECTION('',(-1.,0.,0.));
#16824=DIRECTION('center_axis',(0.,-0.707106781186543,-0.707106781186552));
#16825=DIRECTION('ref_axis',(-1.,0.,0.));
#16826=DIRECTION('',(1.,0.,0.));
#16827=DIRECTION('center_axis',(0.,0.,1.));
#16828=DIRECTION('ref_axis',(1.,0.,0.));
#16829=DIRECTION('',(0.,1.,0.));
#16830=DIRECTION('',(1.,0.,0.));
#16831=DIRECTION('',(0.,1.,0.));
#16832=DIRECTION('center_axis',(-1.,0.,0.));
#16833=DIRECTION('ref_axis',(0.,0.,1.));
#16834=DIRECTION('',(0.,1.,0.));
#16835=DIRECTION('',(0.,0.,1.));
#16836=DIRECTION('center_axis',(-1.,0.,0.));
#16837=DIRECTION('ref_axis',(0.,0.,-1.));
#16838=DIRECTION('center_axis',(-0.707106781186554,-0.707106781186541,0.));
#16839=DIRECTION('ref_axis',(0.,0.,1.));
#16840=DIRECTION('',(-0.577350269189622,0.577350269189632,-0.577350269189624));
#16841=DIRECTION('',(0.,0.,-1.));
#16842=DIRECTION('',(-0.577350269189622,0.577350269189632,0.577350269189623));
#16843=DIRECTION('center_axis',(0.707106781186552,-0.707106781186543,0.));
#16844=DIRECTION('ref_axis',(0.,0.,-1.));
#16845=DIRECTION('',(0.577350269189623,0.577350269189631,0.577350269189623));
#16846=DIRECTION('',(0.,0.,1.));
#16847=DIRECTION('',(-0.577350269189623,-0.577350269189631,0.577350269189623));
#16848=DIRECTION('center_axis',(0.,-0.707106781186543,0.707106781186552));
#16849=DIRECTION('ref_axis',(1.,0.,0.));
#16850=DIRECTION('',(-1.,0.,0.));
#16851=DIRECTION('center_axis',(0.,-0.707106781186543,-0.707106781186552));
#16852=DIRECTION('ref_axis',(-1.,0.,0.));
#16853=DIRECTION('',(1.,0.,0.));
#16854=DIRECTION('center_axis',(0.,0.,1.));
#16855=DIRECTION('ref_axis',(1.,0.,0.));
#16856=DIRECTION('',(0.,1.,0.));
#16857=DIRECTION('',(1.,0.,0.));
#16858=DIRECTION('',(0.,1.,0.));
#16859=DIRECTION('center_axis',(-1.,0.,0.));
#16860=DIRECTION('ref_axis',(0.,0.,1.));
#16861=DIRECTION('',(0.,1.,0.));
#16862=DIRECTION('',(0.,0.,1.));
#16863=DIRECTION('center_axis',(-1.,0.,0.));
#16864=DIRECTION('ref_axis',(0.,0.,-1.));
#16865=DIRECTION('center_axis',(-1.,0.,0.));
#16866=DIRECTION('ref_axis',(0.,0.,-1.));
#16867=DIRECTION('',(-1.,0.,0.));
#16868=DIRECTION('center_axis',(1.,0.,0.));
#16869=DIRECTION('ref_axis',(0.,0.,-1.));
#16870=DIRECTION('center_axis',(-1.,0.,0.));
#16871=DIRECTION('ref_axis',(0.,0.,-1.));
#16872=DIRECTION('',(-1.,0.,0.));
#16873=DIRECTION('center_axis',(1.,0.,0.));
#16874=DIRECTION('ref_axis',(0.,0.,-1.));
#16875=DIRECTION('center_axis',(-1.,0.,0.));
#16876=DIRECTION('ref_axis',(0.,0.,-1.));
#16877=DIRECTION('',(-1.,0.,0.));
#16878=DIRECTION('center_axis',(1.,0.,0.));
#16879=DIRECTION('ref_axis',(0.,0.,-1.));
#16880=DIRECTION('center_axis',(-1.,0.,0.));
#16881=DIRECTION('ref_axis',(0.,0.,-1.));
#16882=DIRECTION('',(-1.,0.,0.));
#16883=DIRECTION('center_axis',(1.,0.,0.));
#16884=DIRECTION('ref_axis',(0.,0.,-1.));
#16885=DIRECTION('center_axis',(-1.,0.,0.));
#16886=DIRECTION('ref_axis',(0.,0.,-1.));
#16887=DIRECTION('',(-1.,0.,0.));
#16888=DIRECTION('center_axis',(0.,0.,-1.));
#16889=DIRECTION('ref_axis',(-1.,0.,0.));
#16890=DIRECTION('',(0.,1.,0.));
#16891=DIRECTION('',(-1.,0.,0.));
#16892=DIRECTION('center_axis',(1.,0.,0.));
#16893=DIRECTION('ref_axis',(0.,0.,-1.));
#16894=DIRECTION('',(0.,0.,-1.));
#16895=DIRECTION('center_axis',(0.,1.,0.));
#16896=DIRECTION('ref_axis',(0.,0.,1.));
#16897=DIRECTION('center_axis',(0.,0.,-1.));
#16898=DIRECTION('ref_axis',(-1.,0.,0.));
#16899=DIRECTION('',(0.,1.,0.));
#16900=DIRECTION('',(-1.,0.,0.));
#16901=DIRECTION('center_axis',(1.,0.,0.));
#16902=DIRECTION('ref_axis',(0.,0.,-1.));
#16903=DIRECTION('',(0.,0.,-1.));
#16904=DIRECTION('center_axis',(0.,1.,0.));
#16905=DIRECTION('ref_axis',(0.,0.,1.));
#16906=DIRECTION('center_axis',(0.,0.,-1.));
#16907=DIRECTION('ref_axis',(-1.,0.,0.));
#16908=DIRECTION('',(0.,1.,0.));
#16909=DIRECTION('',(-1.,0.,0.));
#16910=DIRECTION('center_axis',(1.,0.,0.));
#16911=DIRECTION('ref_axis',(0.,0.,-1.));
#16912=DIRECTION('',(0.,0.,-1.));
#16913=DIRECTION('center_axis',(0.,1.,0.));
#16914=DIRECTION('ref_axis',(0.,0.,1.));
#16915=DIRECTION('center_axis',(0.,0.,-1.));
#16916=DIRECTION('ref_axis',(-1.,0.,0.));
#16917=DIRECTION('',(0.,1.,0.));
#16918=DIRECTION('',(-1.,0.,0.));
#16919=DIRECTION('center_axis',(1.,0.,0.));
#16920=DIRECTION('ref_axis',(0.,0.,-1.));
#16921=DIRECTION('',(0.,0.,-1.));
#16922=DIRECTION('center_axis',(0.,1.,0.));
#16923=DIRECTION('ref_axis',(0.,0.,1.));
#16924=DIRECTION('center_axis',(0.,0.,1.));
#16925=DIRECTION('ref_axis',(-1.,0.,0.));
#16926=DIRECTION('',(0.,-1.,0.));
#16927=DIRECTION('center_axis',(0.,-1.,0.));
#16928=DIRECTION('ref_axis',(-1.,0.,1.11022302462516E-15));
#16929=DIRECTION('center_axis',(0.,1.,0.));
#16930=DIRECTION('ref_axis',(1.,0.,0.));
#16931=DIRECTION('center_axis',(0.,1.,0.));
#16932=DIRECTION('ref_axis',(1.,0.,0.));
#16933=DIRECTION('center_axis',(0.,1.,0.));
#16934=DIRECTION('ref_axis',(1.,0.,0.));
#16935=DIRECTION('center_axis',(0.,0.,-1.));
#16936=DIRECTION('ref_axis',(1.,0.,0.));
#16937=DIRECTION('',(-1.,0.,0.));
#16938=DIRECTION('center_axis',(0.,1.,0.));
#16939=DIRECTION('ref_axis',(1.,0.,0.));
#16940=DIRECTION('center_axis',(0.,1.,0.));
#16941=DIRECTION('ref_axis',(1.,0.,0.));
#16942=DIRECTION('axis',(0.,0.,1.));
#16943=DIRECTION('refdir',(1.,0.,0.));
#16944=DIRECTION('center_axis',(-1.,0.,-9.61370872096891E-16));
#16945=DIRECTION('ref_axis',(0.,-1.,-3.31661110028857E-17));
#16946=DIRECTION('center_axis',(-1.,0.,0.));
#16947=DIRECTION('ref_axis',(0.,-1.,0.));
#16948=DIRECTION('',(-0.38268343236509,0.923879532511287,-2.24116602752525E-16));
#16949=DIRECTION('center_axis',(1.,0.,0.));
#16950=DIRECTION('ref_axis',(0.,-1.,-6.12323399573677E-17));
#16951=DIRECTION('center_axis',(1.,0.,0.));
#16952=DIRECTION('ref_axis',(0.,-1.,-6.12323399573677E-17));
#16953=DIRECTION('center_axis',(-1.,0.,0.));
#16954=DIRECTION('ref_axis',(0.,1.,0.));
#16955=DIRECTION('',(-0.707106781186548,-0.707106781186547,-8.65956056235493E-17));
#16956=DIRECTION('center_axis',(-1.,0.,0.));
#16957=DIRECTION('ref_axis',(0.,-1.,-6.12323399573677E-17));
#16958=DIRECTION('center_axis',(-1.,0.,0.));
#16959=DIRECTION('ref_axis',(0.,-1.,-6.12323399573677E-17));
#16960=DIRECTION('center_axis',(1.,0.,0.));
#16961=DIRECTION('ref_axis',(0.,0.,-1.));
#16962=DIRECTION('center_axis',(-1.,0.,4.23000162973647E-16));
#16963=DIRECTION('ref_axis',(0.,-1.,-2.9725008056928E-17));
#16964=DIRECTION('',(-0.923879532511284,0.382683432365095,4.49041664983859E-16));
#16965=DIRECTION('center_axis',(1.,0.,0.));
#16966=DIRECTION('ref_axis',(0.,-1.,0.));
#16967=DIRECTION('center_axis',(1.,0.,0.));
#16968=DIRECTION('ref_axis',(0.,-1.,0.));
#16969=DIRECTION('center_axis',(1.,0.,0.));
#16970=DIRECTION('ref_axis',(0.,1.,0.));
#16971=DIRECTION('',(-1.,0.,0.));
#16972=DIRECTION('center_axis',(1.,0.,0.));
#16973=DIRECTION('ref_axis',(0.,0.,-1.));
#16974=DIRECTION('center_axis',(-1.,0.,0.));
#16975=DIRECTION('ref_axis',(0.,0.,1.));
#16976=DIRECTION('center_axis',(1.,0.,0.));
#16977=DIRECTION('ref_axis',(0.,0.,-1.));
#16978=DIRECTION('center_axis',(1.,0.,0.));
#16979=DIRECTION('ref_axis',(0.,1.,0.));
#16980=DIRECTION('',(-0.624695047554424,0.78086880944303,9.56288488038411E-17));
#16981=DIRECTION('axis',(0.,0.,1.));
#16982=DIRECTION('refdir',(1.,0.,0.));
#16983=DIRECTION('center_axis',(-1.,0.,0.));
#16984=DIRECTION('ref_axis',(0.,0.,1.));
#16985=DIRECTION('center_axis',(1.,0.,0.));
#16986=DIRECTION('ref_axis',(0.,0.,-1.));
#16987=DIRECTION('center_axis',(1.,0.,0.));
#16988=DIRECTION('ref_axis',(0.,1.,0.));
#16989=DIRECTION('center_axis',(1.,0.,0.));
#16990=DIRECTION('ref_axis',(0.,0.,-1.));
#16991=DIRECTION('',(-0.707106781186547,0.707106781186548,8.65956056235493E-17));
#16992=DIRECTION('center_axis',(1.,0.,0.));
#16993=DIRECTION('ref_axis',(0.,1.,0.));
#16994=DIRECTION('center_axis',(1.,0.,0.));
#16995=DIRECTION('ref_axis',(0.,0.,-1.));
#16996=DIRECTION('',(-1.,0.,0.));
#16997=DIRECTION('center_axis',(-1.,0.,0.));
#16998=DIRECTION('ref_axis',(0.,1.,0.));
#16999=DIRECTION('center_axis',(1.,0.,0.));
#17000=DIRECTION('ref_axis',(0.,0.,-1.));
#17001=DIRECTION('',(-0.707106781186545,-0.70710678118655,-8.65956056235496E-17));
#17002=DIRECTION('center_axis',(1.,0.,0.));
#17003=DIRECTION('ref_axis',(0.,0.,-1.));
#17004=DIRECTION('axis',(0.,0.,1.));
#17005=DIRECTION('refdir',(1.,0.,0.));
#17006=DIRECTION('center_axis',(0.,-0.934100663920609,-0.357009733288993));
#17007=DIRECTION('ref_axis',(0.,0.357009733288993,-0.934100663920609));
#17008=DIRECTION('',(0.,0.357009733288993,-0.934100663920609));
#17009=DIRECTION('',(1.,0.,0.));
#17010=DIRECTION('',(0.,0.357009733288993,-0.934100663920609));
#17011=DIRECTION('',(1.,0.,0.));
#17012=DIRECTION('center_axis',(0.,-0.821646937942163,-0.569996762596303));
#17013=DIRECTION('ref_axis',(0.,0.569996762596303,-0.821646937942163));
#17014=DIRECTION('',(0.,0.569996762596303,-0.821646937942163));
#17015=DIRECTION('',(0.,0.569996762596303,-0.821646937942163));
#17016=DIRECTION('',(1.,0.,0.));
#17017=DIRECTION('center_axis',(0.,-0.661530035807154,-0.749918670073619));
#17018=DIRECTION('ref_axis',(0.,0.749918670073619,-0.661530035807154));
#17019=DIRECTION('',(0.,0.749918670073619,-0.661530035807154));
#17020=DIRECTION('',(0.,0.749918670073619,-0.661530035807154));
#17021=DIRECTION('',(1.,0.,0.));
#17022=DIRECTION('center_axis',(0.,-0.463038229350705,-0.886338309089573));
#17023=DIRECTION('ref_axis',(0.,0.886338309089573,-0.463038229350705));
#17024=DIRECTION('',(0.,0.886338309089573,-0.463038229350705));
#17025=DIRECTION('',(0.,0.886338309089573,-0.463038229350705));
#17026=DIRECTION('',(1.,0.,0.));
#17027=DIRECTION('center_axis',(0.,-0.237685892326173,-0.971342069813262));
#17028=DIRECTION('ref_axis',(0.,0.971342069813261,-0.237685892326173));
#17029=DIRECTION('',(0.,0.971342069813261,-0.237685892326173));
#17030=DIRECTION('',(0.,0.971342069813261,-0.237685892326173));
#17031=DIRECTION('',(1.,0.,0.));
#17032=DIRECTION('center_axis',(0.,0.00145444053054168,-0.999998942300812));
#17033=DIRECTION('ref_axis',(0.,0.999998942300812,0.00145444053054168));
#17034=DIRECTION('',(0.,0.999998942300812,0.00145444053054168));
#17035=DIRECTION('',(0.,0.999998942300812,0.00145444053054168));
#17036=DIRECTION('',(1.,0.,0.));
#17037=DIRECTION('center_axis',(0.,0.240510402288168,-0.970646561005181));
#17038=DIRECTION('ref_axis',(0.,0.97064656100518,0.240510402288168));
#17039=DIRECTION('',(0.,0.97064656100518,0.240510402288168));
#17040=DIRECTION('',(0.,0.97064656100518,0.240510402288168));
#17041=DIRECTION('',(1.,0.,0.));
#17042=DIRECTION('center_axis',(0.,0.465614520325111,-0.884987637463042));
#17043=DIRECTION('ref_axis',(0.,0.884987637463042,0.465614520325111));
#17044=DIRECTION('',(0.,0.884987637463042,0.465614520325111));
#17045=DIRECTION('',(0.,0.884987637463042,0.465614520325111));
#17046=DIRECTION('',(1.,0.,0.));
#17047=DIRECTION('center_axis',(0.,0.663708658918947,-0.74799118716467));
#17048=DIRECTION('ref_axis',(0.,0.74799118716467,0.663708658918947));
#17049=DIRECTION('',(0.,0.74799118716467,0.663708658918947));
#17050=DIRECTION('',(0.,0.74799118716467,0.663708658918947));
#17051=DIRECTION('',(1.,0.,0.));
#17052=DIRECTION('center_axis',(0.,0.82330151275668,-0.567604280368428));
#17053=DIRECTION('ref_axis',(0.,0.567604280368429,0.823301512756681));
#17054=DIRECTION('',(0.,0.567604280368428,0.82330151275668));
#17055=DIRECTION('',(0.,0.567604280368428,0.82330151275668));
#17056=DIRECTION('',(1.,0.,0.));
#17057=DIRECTION('center_axis',(0.,0.935135209686012,-0.354291037997716));
#17058=DIRECTION('ref_axis',(0.,0.354291037997716,0.935135209686012));
#17059=DIRECTION('',(0.,0.354291037997716,0.935135209686012));
#17060=DIRECTION('',(0.,0.354291037997716,0.935135209686012));
#17061=DIRECTION('',(1.,0.,0.));
#17062=DIRECTION('center_axis',(0.,0.992722353538543,-0.120425615152662));
#17063=DIRECTION('ref_axis',(0.,0.120425615152662,0.992722353538542));
#17064=DIRECTION('',(0.,0.120425615152662,0.992722353538542));
#17065=DIRECTION('',(0.,0.120425615152662,0.992722353538542));
#17066=DIRECTION('',(1.,0.,0.));
#17067=DIRECTION('center_axis',(0.,0.992722353538543,0.120425615152661));
#17068=DIRECTION('ref_axis',(0.,-0.120425615152661,0.992722353538543));
#17069=DIRECTION('',(0.,-0.120425615152661,0.992722353538543));
#17070=DIRECTION('',(0.,-0.120425615152661,0.992722353538543));
#17071=DIRECTION('',(1.,0.,0.));
#17072=DIRECTION('center_axis',(0.,0.935135209686012,0.354291037997715));
#17073=DIRECTION('ref_axis',(0.,-0.354291037997715,0.935135209686012));
#17074=DIRECTION('',(0.,-0.354291037997715,0.935135209686012));
#17075=DIRECTION('',(0.,-0.354291037997715,0.935135209686012));
#17076=DIRECTION('',(1.,0.,0.));
#17077=DIRECTION('center_axis',(0.,0.82330151275668,0.567604280368429));
#17078=DIRECTION('ref_axis',(0.,-0.567604280368429,0.82330151275668));
#17079=DIRECTION('',(0.,-0.567604280368429,0.82330151275668));
#17080=DIRECTION('',(0.,-0.567604280368429,0.82330151275668));
#17081=DIRECTION('',(1.,0.,0.));
#17082=DIRECTION('center_axis',(0.,0.663708658918947,0.747991187164671));
#17083=DIRECTION('ref_axis',(0.,-0.747991187164671,0.663708658918947));
#17084=DIRECTION('',(0.,-0.747991187164671,0.663708658918946));
#17085=DIRECTION('',(0.,-0.747991187164671,0.663708658918946));
#17086=DIRECTION('',(1.,0.,0.));
#17087=DIRECTION('center_axis',(0.,0.465614520325111,0.884987637463042));
#17088=DIRECTION('ref_axis',(0.,-0.884987637463042,0.465614520325111));
#17089=DIRECTION('',(0.,-0.884987637463042,0.465614520325111));
#17090=DIRECTION('',(0.,-0.884987637463042,0.465614520325111));
#17091=DIRECTION('',(1.,0.,0.));
#17092=DIRECTION('center_axis',(0.,0.240510402288168,0.97064656100518));
#17093=DIRECTION('ref_axis',(0.,-0.97064656100518,0.240510402288168));
#17094=DIRECTION('',(0.,-0.97064656100518,0.240510402288168));
#17095=DIRECTION('',(0.,-0.97064656100518,0.240510402288168));
#17096=DIRECTION('',(1.,0.,0.));
#17097=DIRECTION('center_axis',(0.,0.00145444053054169,0.999998942300812));
#17098=DIRECTION('ref_axis',(0.,-0.999998942300812,0.00145444053054169));
#17099=DIRECTION('',(0.,-0.999998942300812,0.00145444053054169));
#17100=DIRECTION('',(0.,-0.999998942300812,0.00145444053054169));
#17101=DIRECTION('',(1.,0.,0.));
#17102=DIRECTION('center_axis',(0.,-0.237685892326173,0.971342069813261));
#17103=DIRECTION('ref_axis',(0.,-0.971342069813261,-0.237685892326173));
#17104=DIRECTION('',(0.,-0.971342069813261,-0.237685892326173));
#17105=DIRECTION('',(0.,-0.971342069813261,-0.237685892326173));
#17106=DIRECTION('',(1.,0.,0.));
#17107=DIRECTION('center_axis',(0.,-0.463038229350704,0.886338309089574));
#17108=DIRECTION('ref_axis',(0.,-0.886338309089573,-0.463038229350704));
#17109=DIRECTION('',(0.,-0.886338309089573,-0.463038229350704));
#17110=DIRECTION('',(0.,-0.886338309089573,-0.463038229350704));
#17111=DIRECTION('',(1.,0.,0.));
#17112=DIRECTION('center_axis',(0.,-0.661530035807154,0.749918670073619));
#17113=DIRECTION('ref_axis',(0.,-0.749918670073619,-0.661530035807154));
#17114=DIRECTION('',(0.,-0.749918670073619,-0.661530035807154));
#17115=DIRECTION('',(0.,-0.749918670073619,-0.661530035807154));
#17116=DIRECTION('',(1.,0.,0.));
#17117=DIRECTION('center_axis',(0.,-0.821646937942163,0.569996762596303));
#17118=DIRECTION('ref_axis',(0.,-0.569996762596303,-0.821646937942163));
#17119=DIRECTION('',(0.,-0.569996762596303,-0.821646937942163));
#17120=DIRECTION('',(0.,-0.569996762596303,-0.821646937942163));
#17121=DIRECTION('',(1.,0.,0.));
#17122=DIRECTION('center_axis',(0.,-0.934100663920608,0.357009733288994));
#17123=DIRECTION('ref_axis',(0.,-0.357009733288994,-0.934100663920608));
#17124=DIRECTION('',(0.,-0.357009733288994,-0.934100663920608));
#17125=DIRECTION('',(0.,-0.357009733288994,-0.934100663920608));
#17126=DIRECTION('',(1.,0.,0.));
#17127=DIRECTION('center_axis',(0.,0.241921895599669,0.970295726275996));
#17128=DIRECTION('ref_axis',(0.,-0.970295726275996,0.241921895599669));
#17129=DIRECTION('',(0.,-0.970295726275996,0.241921895599669));
#17130=DIRECTION('',(0.,-0.970295726275996,0.241921895599669));
#17131=DIRECTION('',(1.,0.,0.));
#17132=DIRECTION('center_axis',(0.,0.934100663920609,-0.357009733288994));
#17133=DIRECTION('ref_axis',(0.,0.357009733288994,0.934100663920609));
#17134=DIRECTION('',(0.,0.357009733288994,0.934100663920608));
#17135=DIRECTION('',(0.,0.357009733288994,0.934100663920608));
#17136=DIRECTION('',(1.,0.,0.));
#17137=DIRECTION('center_axis',(0.,0.821646937942163,-0.569996762596304));
#17138=DIRECTION('ref_axis',(0.,0.569996762596304,0.821646937942163));
#17139=DIRECTION('',(0.,0.569996762596304,0.821646937942163));
#17140=DIRECTION('',(0.,0.569996762596304,0.821646937942163));
#17141=DIRECTION('',(1.,0.,0.));
#17142=DIRECTION('center_axis',(0.,0.661530035807154,-0.749918670073619));
#17143=DIRECTION('ref_axis',(0.,0.749918670073619,0.661530035807154));
#17144=DIRECTION('',(0.,0.749918670073619,0.661530035807154));
#17145=DIRECTION('',(0.,0.749918670073619,0.661530035807154));
#17146=DIRECTION('',(1.,0.,0.));
#17147=DIRECTION('center_axis',(0.,0.463038229350705,-0.886338309089573));
#17148=DIRECTION('ref_axis',(0.,0.886338309089573,0.463038229350705));
#17149=DIRECTION('',(0.,0.886338309089573,0.463038229350705));
#17150=DIRECTION('',(0.,0.886338309089573,0.463038229350705));
#17151=DIRECTION('',(1.,0.,0.));
#17152=DIRECTION('center_axis',(0.,0.237685892326173,-0.971342069813261));
#17153=DIRECTION('ref_axis',(0.,0.971342069813261,0.237685892326173));
#17154=DIRECTION('',(0.,0.971342069813261,0.237685892326173));
#17155=DIRECTION('',(0.,0.971342069813261,0.237685892326173));
#17156=DIRECTION('',(1.,0.,0.));
#17157=DIRECTION('center_axis',(0.,-0.00145444053054132,-0.999998942300812));
#17158=DIRECTION('ref_axis',(0.,0.999998942300812,-0.00145444053054132));
#17159=DIRECTION('',(0.,0.999998942300812,-0.00145444053054132));
#17160=DIRECTION('',(0.,0.999998942300812,-0.00145444053054132));
#17161=DIRECTION('',(1.,0.,0.));
#17162=DIRECTION('center_axis',(0.,-0.240510402288168,-0.97064656100518));
#17163=DIRECTION('ref_axis',(0.,0.97064656100518,-0.240510402288168));
#17164=DIRECTION('',(0.,0.97064656100518,-0.240510402288168));
#17165=DIRECTION('',(0.,0.97064656100518,-0.240510402288168));
#17166=DIRECTION('',(1.,0.,0.));
#17167=DIRECTION('center_axis',(0.,-0.465614520325111,-0.884987637463042));
#17168=DIRECTION('ref_axis',(0.,0.884987637463042,-0.465614520325111));
#17169=DIRECTION('',(0.,0.884987637463042,-0.465614520325111));
#17170=DIRECTION('',(0.,0.884987637463042,-0.465614520325111));
#17171=DIRECTION('',(1.,0.,0.));
#17172=DIRECTION('center_axis',(0.,-0.663708658918947,-0.74799118716467));
#17173=DIRECTION('ref_axis',(0.,0.74799118716467,-0.663708658918947));
#17174=DIRECTION('',(0.,0.74799118716467,-0.663708658918947));
#17175=DIRECTION('',(0.,0.74799118716467,-0.663708658918947));
#17176=DIRECTION('',(1.,0.,0.));
#17177=DIRECTION('center_axis',(0.,-0.82330151275668,-0.567604280368429));
#17178=DIRECTION('ref_axis',(0.,0.567604280368429,-0.82330151275668));
#17179=DIRECTION('',(0.,0.567604280368429,-0.82330151275668));
#17180=DIRECTION('',(0.,0.567604280368429,-0.82330151275668));
#17181=DIRECTION('',(1.,0.,0.));
#17182=DIRECTION('center_axis',(0.,-0.935135209686012,-0.354291037997715));
#17183=DIRECTION('ref_axis',(0.,0.354291037997715,-0.935135209686012));
#17184=DIRECTION('',(0.,0.354291037997715,-0.935135209686012));
#17185=DIRECTION('',(0.,0.354291037997715,-0.935135209686012));
#17186=DIRECTION('',(1.,0.,0.));
#17187=DIRECTION('center_axis',(0.,-0.992722353538543,-0.120425615152661));
#17188=DIRECTION('ref_axis',(0.,0.120425615152661,-0.992722353538542));
#17189=DIRECTION('',(0.,0.120425615152661,-0.992722353538543));
#17190=DIRECTION('',(0.,0.120425615152661,-0.992722353538543));
#17191=DIRECTION('',(1.,0.,0.));
#17192=DIRECTION('center_axis',(0.,-0.992722353538543,0.120425615152662));
#17193=DIRECTION('ref_axis',(0.,-0.120425615152662,-0.992722353538542));
#17194=DIRECTION('',(0.,-0.120425615152662,-0.992722353538542));
#17195=DIRECTION('',(0.,-0.120425615152662,-0.992722353538542));
#17196=DIRECTION('',(1.,0.,0.));
#17197=DIRECTION('center_axis',(0.,-0.935135209686012,0.354291037997716));
#17198=DIRECTION('ref_axis',(0.,-0.354291037997716,-0.935135209686012));
#17199=DIRECTION('',(0.,-0.354291037997716,-0.935135209686012));
#17200=DIRECTION('',(0.,-0.354291037997716,-0.935135209686012));
#17201=DIRECTION('',(1.,0.,0.));
#17202=DIRECTION('center_axis',(0.,-0.82330151275668,0.567604280368429));
#17203=DIRECTION('ref_axis',(0.,-0.567604280368429,-0.82330151275668));
#17204=DIRECTION('',(0.,-0.567604280368429,-0.82330151275668));
#17205=DIRECTION('',(0.,-0.567604280368429,-0.82330151275668));
#17206=DIRECTION('',(1.,0.,0.));
#17207=DIRECTION('center_axis',(0.,-0.663708658918947,0.74799118716467));
#17208=DIRECTION('ref_axis',(0.,-0.74799118716467,-0.663708658918947));
#17209=DIRECTION('',(0.,-0.74799118716467,-0.663708658918947));
#17210=DIRECTION('',(0.,-0.74799118716467,-0.663708658918947));
#17211=DIRECTION('',(1.,0.,0.));
#17212=DIRECTION('center_axis',(0.,-0.465614520325111,0.884987637463042));
#17213=DIRECTION('ref_axis',(0.,-0.884987637463042,-0.465614520325111));
#17214=DIRECTION('',(0.,-0.884987637463042,-0.465614520325111));
#17215=DIRECTION('',(0.,-0.884987637463042,-0.465614520325111));
#17216=DIRECTION('',(1.,0.,0.));
#17217=DIRECTION('center_axis',(0.,-0.240510402288169,0.97064656100518));
#17218=DIRECTION('ref_axis',(0.,-0.97064656100518,-0.240510402288169));
#17219=DIRECTION('',(0.,-0.97064656100518,-0.240510402288169));
#17220=DIRECTION('',(0.,-0.97064656100518,-0.240510402288169));
#17221=DIRECTION('',(1.,0.,0.));
#17222=DIRECTION('center_axis',(0.,-0.00145444053054131,0.999998942300812));
#17223=DIRECTION('ref_axis',(0.,-0.999998942300812,-0.00145444053054131));
#17224=DIRECTION('',(0.,-0.999998942300812,-0.00145444053054131));
#17225=DIRECTION('',(0.,-0.999998942300812,-0.00145444053054131));
#17226=DIRECTION('',(1.,0.,0.));
#17227=DIRECTION('center_axis',(0.,0.237685892326173,0.971342069813262));
#17228=DIRECTION('ref_axis',(0.,-0.971342069813262,0.237685892326173));
#17229=DIRECTION('',(0.,-0.971342069813262,0.237685892326173));
#17230=DIRECTION('',(0.,-0.971342069813262,0.237685892326173));
#17231=DIRECTION('',(1.,0.,0.));
#17232=DIRECTION('center_axis',(0.,0.463038229350705,0.886338309089573));
#17233=DIRECTION('ref_axis',(0.,-0.886338309089573,0.463038229350705));
#17234=DIRECTION('',(0.,-0.886338309089573,0.463038229350705));
#17235=DIRECTION('',(0.,-0.886338309089573,0.463038229350705));
#17236=DIRECTION('',(1.,0.,0.));
#17237=DIRECTION('center_axis',(0.,0.661530035807154,0.749918670073619));
#17238=DIRECTION('ref_axis',(0.,-0.749918670073619,0.661530035807154));
#17239=DIRECTION('',(0.,-0.749918670073619,0.661530035807154));
#17240=DIRECTION('',(0.,-0.749918670073619,0.661530035807154));
#17241=DIRECTION('',(1.,0.,0.));
#17242=DIRECTION('center_axis',(0.,0.821646937942164,0.569996762596303));
#17243=DIRECTION('ref_axis',(0.,-0.569996762596303,0.821646937942164));
#17244=DIRECTION('',(0.,-0.569996762596303,0.821646937942164));
#17245=DIRECTION('',(0.,-0.569996762596303,0.821646937942164));
#17246=DIRECTION('',(1.,0.,0.));
#17247=DIRECTION('center_axis',(0.,0.934100663920609,0.357009733288993));
#17248=DIRECTION('ref_axis',(0.,-0.357009733288993,0.934100663920609));
#17249=DIRECTION('',(0.,-0.357009733288993,0.934100663920609));
#17250=DIRECTION('',(0.,-0.357009733288993,0.934100663920609));
#17251=DIRECTION('',(1.,0.,0.));
#17252=DIRECTION('center_axis',(0.,0.241921895599668,-0.970295726275996));
#17253=DIRECTION('ref_axis',(0.,0.970295726275996,0.241921895599668));
#17254=DIRECTION('',(0.,0.970295726275996,0.241921895599668));
#17255=DIRECTION('',(0.,0.970295726275996,0.241921895599668));
#17256=DIRECTION('center_axis',(1.,0.,0.));
#17257=DIRECTION('ref_axis',(0.,0.,-1.));
#17258=DIRECTION('center_axis',(1.,0.,0.));
#17259=DIRECTION('ref_axis',(0.,0.,-1.));
#17260=DIRECTION('axis',(0.,0.,1.));
#17261=DIRECTION('refdir',(1.,0.,0.));
#17262=DIRECTION('center_axis',(0.707106781186545,0.70710678118655,0.));
#17263=DIRECTION('ref_axis',(0.,0.,-1.));
#17264=DIRECTION('',(-0.70710678118655,0.707106781186545,0.));
#17265=DIRECTION('',(0.,0.,1.));
#17266=DIRECTION('',(0.70710678118655,-0.707106781186545,-7.85046229341888E-16));
#17267=DIRECTION('',(0.,0.,-1.));
#17268=DIRECTION('center_axis',(0.,1.,0.));
#17269=DIRECTION('ref_axis',(-3.96508223080413E-16,0.,-1.));
#17270=DIRECTION('',(-3.92523114670943E-16,0.707106781186544,-0.707106781186551));
#17271=DIRECTION('center_axis',(0.,1.,0.));
#17272=DIRECTION('ref_axis',(-3.96508223080413E-16,0.,-1.));
#17273=DIRECTION('center_axis',(0.,-1.,0.));
#17274=DIRECTION('ref_axis',(-3.96508223080413E-16,0.,-1.));
#17275=DIRECTION('center_axis',(0.,0.707106781186549,0.707106781186546));
#17276=DIRECTION('ref_axis',(1.,0.,0.));
#17277=DIRECTION('',(0.,0.707106781186546,-0.707106781186549));
#17278=DIRECTION('',(-1.,0.,0.));
#17279=DIRECTION('',(1.,0.,0.));
#17280=DIRECTION('center_axis',(0.,1.,0.));
#17281=DIRECTION('ref_axis',(1.,0.,-9.51619735392991E-16));
#17282=DIRECTION('',(0.707106781186548,0.707106781186548,-7.8504622934189E-16));
#17283=DIRECTION('center_axis',(0.,1.,0.));
#17284=DIRECTION('ref_axis',(1.,0.,-9.51619735392991E-16));
#17285=DIRECTION('center_axis',(0.,-1.,0.));
#17286=DIRECTION('ref_axis',(1.,0.,-9.51619735392991E-16));
#17287=DIRECTION('center_axis',(-0.707106781186548,0.707106781186548,0.));
#17288=DIRECTION('ref_axis',(0.,0.,1.));
#17289=DIRECTION('',(0.707106781186548,0.707106781186548,0.));
#17290=DIRECTION('',(0.,0.,-1.));
#17291=DIRECTION('',(0.,0.,1.));
#17292=DIRECTION('center_axis',(0.,1.,0.));
#17293=DIRECTION('ref_axis',(6.3441315692866E-16,0.,1.));
#17294=DIRECTION('',(0.,0.707106781186546,0.707106781186549));
#17295=DIRECTION('center_axis',(0.,1.,0.));
#17296=DIRECTION('ref_axis',(6.3441315692866E-16,0.,1.));
#17297=DIRECTION('center_axis',(0.,-1.,0.));
#17298=DIRECTION('ref_axis',(6.3441315692866E-16,0.,1.));
#17299=DIRECTION('center_axis',(0.,0.707106781186549,-0.707106781186546));
#17300=DIRECTION('ref_axis',(-1.,0.,0.));
#17301=DIRECTION('',(3.92523114670944E-16,0.707106781186546,0.707106781186549));
#17302=DIRECTION('',(1.,0.,0.));
#17303=DIRECTION('',(-1.,0.,0.));
#17304=DIRECTION('center_axis',(0.,1.,0.));
#17305=DIRECTION('ref_axis',(-1.,0.,3.1720657846433E-16));
#17306=DIRECTION('center_axis',(0.,1.,0.));
#17307=DIRECTION('ref_axis',(-1.,0.,3.1720657846433E-16));
#17308=DIRECTION('center_axis',(0.,-1.,0.));
#17309=DIRECTION('ref_axis',(-1.,0.,3.1720657846433E-16));
#17310=DIRECTION('center_axis',(0.,-1.,0.));
#17311=DIRECTION('ref_axis',(1.,0.,-9.51619735392991E-16));
#17312=DIRECTION('',(0.,-1.,0.));
#17313=DIRECTION('center_axis',(0.,1.,0.));
#17314=DIRECTION('ref_axis',(1.,0.,-9.51619735392991E-16));
#17315=DIRECTION('',(0.,-1.,0.));
#17316=DIRECTION('center_axis',(0.,0.,1.));
#17317=DIRECTION('ref_axis',(-1.,0.,0.));
#17318=DIRECTION('',(0.,-1.,0.));
#17319=DIRECTION('',(-1.,0.,0.));
#17320=DIRECTION('center_axis',(0.,-1.,0.));
#17321=DIRECTION('ref_axis',(-3.96508223080413E-16,0.,-1.));
#17322=DIRECTION('',(0.,-1.,0.));
#17323=DIRECTION('center_axis',(0.,1.,0.));
#17324=DIRECTION('ref_axis',(-3.96508223080413E-16,0.,-1.));
#17325=DIRECTION('center_axis',(1.,0.,0.));
#17326=DIRECTION('ref_axis',(0.,0.,1.));
#17327=DIRECTION('',(0.,-1.,0.));
#17328=DIRECTION('',(0.,0.,1.));
#17329=DIRECTION('center_axis',(0.,1.,0.));
#17330=DIRECTION('ref_axis',(1.,0.,0.));
#17331=DIRECTION('',(0.,0.,1.));
#17332=DIRECTION('center_axis',(0.,-1.,0.));
#17333=DIRECTION('ref_axis',(1.,0.,0.));
#17334=DIRECTION('',(1.,0.,0.));
#17335=DIRECTION('center_axis',(0.,-1.,0.));
#17336=DIRECTION('ref_axis',(-6.5658350918692E-16,0.,-1.));
#17337=DIRECTION('',(0.,0.,-1.));
#17338=DIRECTION('center_axis',(0.,-1.,0.));
#17339=DIRECTION('ref_axis',(-1.,0.,5.96894099260836E-16));
#17340=DIRECTION('',(-1.,0.,0.));
#17341=DIRECTION('center_axis',(0.,-1.,0.));
#17342=DIRECTION('ref_axis',(4.7751527940867E-16,0.,1.));
#17343=DIRECTION('center_axis',(0.,1.,0.));
#17344=DIRECTION('ref_axis',(1.,0.,0.));
#17345=DIRECTION('',(0.707106781186548,0.707106781186548,0.));
#17346=DIRECTION('center_axis',(0.,1.,0.));
#17347=DIRECTION('ref_axis',(1.,0.,0.));
#17348=DIRECTION('',(0.,-0.707106781186544,0.707106781186551));
#17349=DIRECTION('center_axis',(0.,-1.,0.));
#17350=DIRECTION('ref_axis',(1.,0.,0.));
#17351=DIRECTION('center_axis',(-0.707106781186548,0.707106781186548,0.));
#17352=DIRECTION('ref_axis',(0.,0.,1.));
#17353=DIRECTION('',(0.707106781186551,0.707106781186544,0.));
#17354=DIRECTION('',(0.,0.,-1.));
#17355=DIRECTION('',(0.,0.,1.));
#17356=DIRECTION('center_axis',(0.,1.,0.));
#17357=DIRECTION('ref_axis',(4.7751527940867E-16,0.,1.));
#17358=DIRECTION('',(0.,0.707106781186548,0.707106781186548));
#17359=DIRECTION('center_axis',(0.,1.,0.));
#17360=DIRECTION('ref_axis',(4.7751527940867E-16,0.,1.));
#17361=DIRECTION('center_axis',(0.,-1.,0.));
#17362=DIRECTION('ref_axis',(4.7751527940867E-16,0.,1.));
#17363=DIRECTION('center_axis',(0.,0.707106781186549,-0.707106781186546));
#17364=DIRECTION('ref_axis',(-1.,0.,0.));
#17365=DIRECTION('',(-3.92523114670944E-16,0.707106781186546,0.707106781186549));
#17366=DIRECTION('',(1.,0.,0.));
#17367=DIRECTION('',(-1.,0.,0.));
#17368=DIRECTION('center_axis',(0.,1.,0.));
#17369=DIRECTION('ref_axis',(-1.,0.,5.96894099260837E-16));
#17370=DIRECTION('',(-0.707106781186548,0.707106781186547,7.85046229341889E-16));
#17371=DIRECTION('center_axis',(0.,1.,0.));
#17372=DIRECTION('ref_axis',(-1.,0.,5.96894099260836E-16));
#17373=DIRECTION('center_axis',(0.,-1.,0.));
#17374=DIRECTION('ref_axis',(-1.,0.,5.96894099260836E-16));
#17375=DIRECTION('center_axis',(0.707106781186547,0.707106781186548,0.));
#17376=DIRECTION('ref_axis',(0.,0.,-1.));
#17377=DIRECTION('',(-0.707106781186548,0.707106781186547,0.));
#17378=DIRECTION('',(0.,0.,1.));
#17379=DIRECTION('',(0.,0.,-1.));
#17380=DIRECTION('center_axis',(0.,1.,0.));
#17381=DIRECTION('ref_axis',(-6.5658350918692E-16,0.,-1.));
#17382=DIRECTION('',(-3.92523114670945E-16,0.707106781186548,-0.707106781186548));
#17383=DIRECTION('center_axis',(0.,1.,0.));
#17384=DIRECTION('ref_axis',(-6.5658350918692E-16,0.,-1.));
#17385=DIRECTION('center_axis',(0.,-1.,0.));
#17386=DIRECTION('ref_axis',(-6.5658350918692E-16,0.,-1.));
#17387=DIRECTION('center_axis',(0.,0.707106781186549,0.707106781186546));
#17388=DIRECTION('ref_axis',(1.,0.,0.));
#17389=DIRECTION('',(-1.,0.,0.));
#17390=DIRECTION('',(1.,0.,0.));
#17391=DIRECTION('center_axis',(0.,0.,-1.));
#17392=DIRECTION('ref_axis',(1.,0.,0.));
#17393=DIRECTION('',(0.,-1.,0.));
#17394=DIRECTION('',(0.,-1.,0.));
#17395=DIRECTION('center_axis',(0.,-1.,0.));
#17396=DIRECTION('ref_axis',(4.7751527940867E-16,0.,1.));
#17397=DIRECTION('',(0.,-1.,0.));
#17398=DIRECTION('center_axis',(-1.,0.,0.));
#17399=DIRECTION('ref_axis',(0.,0.,-1.));
#17400=DIRECTION('',(0.,-1.,0.));
#17401=DIRECTION('center_axis',(0.,-1.,0.));
#17402=DIRECTION('ref_axis',(1.,0.,0.));
#17403=DIRECTION('',(0.,-1.,0.));
#17404=DIRECTION('center_axis',(0.,1.,0.));
#17405=DIRECTION('ref_axis',(1.,0.,0.));
#17406=DIRECTION('center_axis',(0.,-1.,0.));
#17407=DIRECTION('ref_axis',(1.26882631385732E-15,0.,1.));
#17408=DIRECTION('',(0.,0.,1.));
#17409=DIRECTION('center_axis',(0.,-1.,0.));
#17410=DIRECTION('ref_axis',(1.,0.,-1.26882631385732E-15));
#17411=DIRECTION('',(1.,0.,0.));
#17412=DIRECTION('center_axis',(0.,-1.,0.));
#17413=DIRECTION('ref_axis',(-9.51619735392991E-16,0.,-1.));
#17414=DIRECTION('',(0.,0.,-1.));
#17415=DIRECTION('center_axis',(0.,-1.,0.));
#17416=DIRECTION('ref_axis',(-1.,0.,6.3441315692866E-16));
#17417=DIRECTION('',(-1.,0.,0.));
#17418=DIRECTION('center_axis',(0.,-1.,0.));
#17419=DIRECTION('ref_axis',(1.26882631385732E-15,0.,1.));
#17420=DIRECTION('',(-0.707106781186548,0.707106781186548,0.));
#17421=DIRECTION('',(0.,-0.707106781186548,0.707106781186548));
#17422=DIRECTION('center_axis',(0.,1.,0.));
#17423=DIRECTION('ref_axis',(1.26882631385732E-15,0.,1.));
#17424=DIRECTION('center_axis',(0.707106781186548,0.707106781186548,0.));
#17425=DIRECTION('ref_axis',(0.,0.,-1.));
#17426=DIRECTION('',(0.,0.,-1.));
#17427=DIRECTION('',(-0.707106781186548,0.707106781186548,0.));
#17428=DIRECTION('center_axis',(0.,-1.,0.));
#17429=DIRECTION('ref_axis',(1.,0.,-1.26882631385732E-15));
#17430=DIRECTION('',(0.,0.707106781186548,0.707106781186548));
#17431=DIRECTION('center_axis',(0.,1.,0.));
#17432=DIRECTION('ref_axis',(1.,0.,-1.26882631385732E-15));
#17433=DIRECTION('center_axis',(0.,0.707106781186548,-0.707106781186548));
#17434=DIRECTION('ref_axis',(-1.,0.,0.));
#17435=DIRECTION('',(-1.,0.,0.));
#17436=DIRECTION('',(1.57009245868378E-15,0.707106781186548,0.707106781186548));
#17437=DIRECTION('center_axis',(0.,-1.,0.));
#17438=DIRECTION('ref_axis',(-9.5161973539299E-16,0.,-1.));
#17439=DIRECTION('',(0.707106781186551,0.707106781186544,3.14018491736755E-15));
#17440=DIRECTION('center_axis',(0.,1.,0.));
#17441=DIRECTION('ref_axis',(-9.51619735392991E-16,0.,-1.));
#17442=DIRECTION('center_axis',(-0.707106781186546,0.707106781186549,0.));
#17443=DIRECTION('ref_axis',(0.,0.,1.));
#17444=DIRECTION('',(0.,0.,1.));
#17445=DIRECTION('',(0.707106781186549,0.707106781186546,0.));
#17446=DIRECTION('center_axis',(0.,-1.,0.));
#17447=DIRECTION('ref_axis',(-1.,0.,6.3441315692866E-16));
#17448=DIRECTION('',(0.,0.707106781186548,-0.707106781186548));
#17449=DIRECTION('center_axis',(0.,1.,0.));
#17450=DIRECTION('ref_axis',(-1.,0.,6.3441315692866E-16));
#17451=DIRECTION('center_axis',(0.,0.707106781186548,0.707106781186548));
#17452=DIRECTION('ref_axis',(1.,0.,0.));
#17453=DIRECTION('',(1.,0.,0.));
#17454=DIRECTION('center_axis',(0.,0.,-1.));
#17455=DIRECTION('ref_axis',(1.,0.,0.));
#17456=DIRECTION('',(0.,-1.,0.));
#17457=DIRECTION('',(0.907485212973028,0.420084025208408,0.));
#17458=DIRECTION('',(1.,0.,0.));
#17459=DIRECTION('',(0.907485212973032,-0.420084025208399,0.));
#17460=DIRECTION('',(0.,-1.,0.));
#17461=DIRECTION('center_axis',(0.,-1.,0.));
#17462=DIRECTION('ref_axis',(1.,0.,-1.26882631385732E-15));
#17463=DIRECTION('',(0.,-1.,0.));
#17464=DIRECTION('center_axis',(0.,-1.,0.));
#17465=DIRECTION('ref_axis',(1.,0.,-1.26882631385732E-15));
#17466=DIRECTION('center_axis',(1.,0.,0.));
#17467=DIRECTION('ref_axis',(0.,0.,1.));
#17468=DIRECTION('',(0.,-1.,0.));
#17469=DIRECTION('',(0.,0.42008402520841,0.907485212973027));
#17470=DIRECTION('',(0.,0.,1.));
#17471=DIRECTION('',(0.,-0.420084025208404,0.90748521297303));
#17472=DIRECTION('center_axis',(0.,-1.,0.));
#17473=DIRECTION('ref_axis',(1.26882631385732E-15,0.,1.));
#17474=DIRECTION('',(0.,-1.,0.));
#17475=DIRECTION('center_axis',(0.,-1.,0.));
#17476=DIRECTION('ref_axis',(1.26882631385732E-15,0.,1.));
#17477=DIRECTION('',(0.,0.420084025208396,-0.907485212973033));
#17478=DIRECTION('',(0.499919264427449,-0.739339319775861,0.451063298537672));
#17479=DIRECTION('center_axis',(0.,1.,0.));
#17480=DIRECTION('ref_axis',(-9.5161973539299E-16,0.,-1.));
#17481=DIRECTION('',(0.437408882639852,-0.707106781186545,0.55558389950372));
#17482=DIRECTION('center_axis',(0.,1.,0.));
#17483=DIRECTION('ref_axis',(-9.51619735392991E-16,0.,-1.));
#17484=DIRECTION('',(-0.555583899503719,0.707106781186547,-0.43740888263985));
#17485=DIRECTION('center_axis',(0.,-1.,0.));
#17486=DIRECTION('ref_axis',(-9.51619735392991E-16,0.,-1.));
#17487=DIRECTION('',(-0.451063298380524,0.739339319957295,-0.499919264300915));
#17488=DIRECTION('center_axis',(1.,0.,0.));
#17489=DIRECTION('ref_axis',(0.,-0.70710678118655,-0.707106781186545));
#17490=DIRECTION('',(-1.,0.,0.));
#17491=DIRECTION('center_axis',(0.,-1.,0.));
#17492=DIRECTION('ref_axis',(-9.51619735392991E-16,0.,-1.));
#17493=DIRECTION('',(0.,-1.,0.));
#17494=DIRECTION('',(0.,-0.420084025208414,-0.907485212973025));
#17495=DIRECTION('',(-0.907485212973031,0.420084025208401,0.));
#17496=DIRECTION('',(0.451063298380521,-0.739339319957302,-0.499919264300906));
#17497=DIRECTION('center_axis',(0.,1.,0.));
#17498=DIRECTION('ref_axis',(-1.,0.,6.3441315692866E-16));
#17499=DIRECTION('',(0.555583899503716,-0.707106781186546,-0.437408882639856));
#17500=DIRECTION('center_axis',(0.,1.,0.));
#17501=DIRECTION('ref_axis',(-1.,0.,6.3441315692866E-16));
#17502=DIRECTION('',(-0.437408882639855,0.707106781186547,0.555583899503715));
#17503=DIRECTION('center_axis',(0.,-1.,0.));
#17504=DIRECTION('ref_axis',(-1.,0.,6.3441315692866E-16));
#17505=DIRECTION('',(-0.499919264427448,0.739339319775853,0.451063298537686));
#17506=DIRECTION('center_axis',(0.,0.,-1.));
#17507=DIRECTION('ref_axis',(-0.707106781186546,-0.707106781186549,0.));
#17508=DIRECTION('',(0.,0.,1.));
#17509=DIRECTION('',(0.,0.,-1.));
#17510=DIRECTION('center_axis',(-1.,0.,0.));
#17511=DIRECTION('ref_axis',(0.,0.,-1.));
#17512=DIRECTION('',(0.,-1.,0.));
#17513=DIRECTION('center_axis',(0.,-1.,0.));
#17514=DIRECTION('ref_axis',(-1.,0.,6.3441315692866E-16));
#17515=DIRECTION('',(0.,-1.,0.));
#17516=DIRECTION('center_axis',(0.,-1.,0.));
#17517=DIRECTION('ref_axis',(1.,0.,-9.51619735392991E-16));
#17518=DIRECTION('',(0.,-0.707106781186548,-0.707106781186548));
#17519=DIRECTION('center_axis',(0.,-1.,0.));
#17520=DIRECTION('ref_axis',(1.,0.,-9.51619735392991E-16));
#17521=DIRECTION('',(-0.707106781186548,0.707106781186548,7.8504622934189E-16));
#17522=DIRECTION('center_axis',(0.,-0.707106781186549,0.707106781186546));
#17523=DIRECTION('ref_axis',(1.,0.,0.));
#17524=DIRECTION('',(7.85046229341889E-16,-0.707106781186546,-0.707106781186549));
#17525=DIRECTION('',(1.,0.,0.));
#17526=DIRECTION('center_axis',(0.,-1.,0.));
#17527=DIRECTION('ref_axis',(-3.96508223080413E-16,0.,-1.));
#17528=DIRECTION('',(-0.70710678118655,-0.707106781186545,-7.85046229341888E-16));
#17529=DIRECTION('center_axis',(0.,-1.,0.));
#17530=DIRECTION('ref_axis',(-3.96508223080413E-16,0.,-1.));
#17531=DIRECTION('center_axis',(0.707106781186547,-0.707106781186548,0.));
#17532=DIRECTION('ref_axis',(0.,0.,-1.));
#17533=DIRECTION('',(-0.707106781186548,-0.707106781186547,7.85046229341889E-16));
#17534=DIRECTION('',(0.,0.,-1.));
#17535=DIRECTION('center_axis',(0.,-1.,0.));
#17536=DIRECTION('ref_axis',(-1.,0.,3.1720657846433E-16));
#17537=DIRECTION('',(-3.92523114670943E-16,-0.707106781186544,0.707106781186551));
#17538=DIRECTION('center_axis',(0.,-1.,0.));
#17539=DIRECTION('ref_axis',(-1.,0.,3.1720657846433E-16));
#17540=DIRECTION('center_axis',(0.,1.,0.));
#17541=DIRECTION('ref_axis',(-1.,0.,3.1720657846433E-16));
#17542=DIRECTION('center_axis',(0.,-0.707106781186549,-0.707106781186546));
#17543=DIRECTION('ref_axis',(-1.,0.,0.));
#17544=DIRECTION('',(0.,-0.707106781186546,0.707106781186549));
#17545=DIRECTION('',(-1.,0.,0.));
#17546=DIRECTION('',(1.,0.,0.));
#17547=DIRECTION('center_axis',(0.,-1.,0.));
#17548=DIRECTION('ref_axis',(6.3441315692866E-16,0.,1.));
#17549=DIRECTION('',(0.707106781186551,-0.707106781186544,7.85046229341887E-16));
#17550=DIRECTION('center_axis',(0.,-1.,0.));
#17551=DIRECTION('ref_axis',(6.3441315692866E-16,0.,1.));
#17552=DIRECTION('center_axis',(0.,1.,0.));
#17553=DIRECTION('ref_axis',(6.3441315692866E-16,0.,1.));
#17554=DIRECTION('center_axis',(-0.707106781186548,-0.707106781186548,0.));
#17555=DIRECTION('ref_axis',(0.,0.,1.));
#17556=DIRECTION('',(0.,0.,1.));
#17557=DIRECTION('',(0.,0.,-1.));
#17558=DIRECTION('center_axis',(0.,1.,0.));
#17559=DIRECTION('ref_axis',(1.,0.,0.));
#17560=DIRECTION('center_axis',(0.,1.,0.));
#17561=DIRECTION('ref_axis',(1.,0.,-1.26882631385732E-15));
#17562=DIRECTION('',(0.,0.,-1.));
#17563=DIRECTION('center_axis',(0.,1.,0.));
#17564=DIRECTION('ref_axis',(1.26882631385732E-15,0.,1.));
#17565=DIRECTION('',(1.,0.,0.));
#17566=DIRECTION('',(-0.451063298380529,-0.739339319957298,0.499919264300905));
#17567=DIRECTION('center_axis',(0.,1.,0.));
#17568=DIRECTION('ref_axis',(1.,0.,-1.26882631385732E-15));
#17569=DIRECTION('',(-0.555583899503719,-0.707106781186544,0.437408882639855));
#17570=DIRECTION('',(0.437408882639851,0.707106781186548,-0.555583899503717));
#17571=DIRECTION('',(0.499919264427449,0.739339319775855,-0.451063298537682));
#17572=DIRECTION('center_axis',(0.,0.,1.));
#17573=DIRECTION('ref_axis',(0.707106781186548,-0.707106781186548,0.));
#17574=DIRECTION('',(-0.907485212973031,-0.420084025208402,0.));
#17575=DIRECTION('',(-0.49991926442746,-0.739339319775848,-0.451063298537683));
#17576=DIRECTION('center_axis',(0.,1.,0.));
#17577=DIRECTION('ref_axis',(1.26882631385732E-15,0.,1.));
#17578=DIRECTION('',(-0.437408882639856,-0.707106781186546,-0.555583899503715));
#17579=DIRECTION('',(0.555583899503722,0.707106781186548,0.437408882639845));
#17580=DIRECTION('',(0.451063298380523,0.739339319957298,0.499919264300911));
#17581=DIRECTION('center_axis',(-1.,0.,0.));
#17582=DIRECTION('ref_axis',(0.,-0.70710678118655,0.707106781186545));
#17583=DIRECTION('',(-1.,0.,0.));
#17584=DIRECTION('center_axis',(0.,0.,1.));
#17585=DIRECTION('ref_axis',(-1.,0.,0.));
#17586=DIRECTION('center_axis',(-1.,0.,0.));
#17587=DIRECTION('ref_axis',(0.,0.,-1.));
#17588=DIRECTION('',(0.,-1.,0.));
#17589=DIRECTION('center_axis',(0.,-1.,0.));
#17590=DIRECTION('ref_axis',(6.3441315692866E-16,0.,1.));
#17591=DIRECTION('',(0.,-1.,0.));
#17592=DIRECTION('center_axis',(0.,0.,-1.));
#17593=DIRECTION('ref_axis',(1.,0.,0.));
#17594=DIRECTION('',(0.,-1.,0.));
#17595=DIRECTION('center_axis',(0.,-1.,0.));
#17596=DIRECTION('ref_axis',(-1.,0.,3.1720657846433E-16));
#17597=DIRECTION('center_axis',(1.,0.,0.));
#17598=DIRECTION('ref_axis',(0.,0.,1.));
#17599=DIRECTION('',(0.,-1.,0.));
#17600=DIRECTION('',(0.,-1.,0.));
#17601=DIRECTION('center_axis',(0.,-1.,0.));
#17602=DIRECTION('ref_axis',(-6.5658350918692E-16,0.,-1.));
#17603=DIRECTION('',(0.,-1.,0.));
#17604=DIRECTION('center_axis',(0.,0.,1.));
#17605=DIRECTION('ref_axis',(-1.,0.,0.));
#17606=DIRECTION('center_axis',(0.,-1.,0.));
#17607=DIRECTION('ref_axis',(-1.,0.,5.96894099260836E-16));
#17608=DIRECTION('axis',(0.,0.,1.));
#17609=DIRECTION('refdir',(1.,0.,0.));
#17610=DIRECTION('center_axis',(0.,0.707106781186548,0.707106781186548));
#17611=DIRECTION('ref_axis',(1.,0.,0.));
#17612=DIRECTION('',(0.,-0.707106781186548,0.707106781186548));
#17613=DIRECTION('',(1.,0.,0.));
#17614=DIRECTION('',(1.,0.,0.));
#17615=DIRECTION('',(1.,0.,0.));
#17616=DIRECTION('',(0.,0.707106781186548,-0.707106781186548));
#17617=DIRECTION('',(-1.,0.,0.));
#17618=DIRECTION('center_axis',(0.,0.,1.));
#17619=DIRECTION('ref_axis',(-1.,-1.97372982155583E-15,0.));
#17620=DIRECTION('',(-0.707106781186549,0.,0.707106781186546));
#17621=DIRECTION('center_axis',(0.,0.,1.));
#17622=DIRECTION('ref_axis',(-1.,-1.97372982155583E-15,0.));
#17623=DIRECTION('center_axis',(0.,0.,-1.));
#17624=DIRECTION('ref_axis',(-1.,-1.97372982155583E-15,0.));
#17625=DIRECTION('center_axis',(0.707106781186549,0.,0.707106781186546));
#17626=DIRECTION('ref_axis',(0.707106781186546,0.,-0.707106781186549));
#17627=DIRECTION('',(-0.707106781186546,0.,0.707106781186549));
#17628=DIRECTION('',(0.,-1.,0.));
#17629=DIRECTION('',(0.,1.,0.));
#17630=DIRECTION('center_axis',(0.,0.,1.));
#17631=DIRECTION('ref_axis',(-2.46716227694479E-15,1.,0.));
#17632=DIRECTION('',(-1.57009245868378E-15,0.707106781186548,0.707106781186548));
#17633=DIRECTION('center_axis',(0.,0.,1.));
#17634=DIRECTION('ref_axis',(-2.46716227694479E-15,1.,0.));
#17635=DIRECTION('center_axis',(0.,0.,-1.));
#17636=DIRECTION('ref_axis',(-2.46716227694479E-15,1.,0.));
#17637=DIRECTION('center_axis',(0.,-0.707106781186551,0.707106781186544));
#17638=DIRECTION('ref_axis',(1.,0.,0.));
#17639=DIRECTION('',(0.,0.707106781186544,0.707106781186551));
#17640=DIRECTION('',(-1.,0.,0.));
#17641=DIRECTION('',(1.,0.,0.));
#17642=DIRECTION('center_axis',(0.,0.,1.));
#17643=DIRECTION('ref_axis',(1.,3.94745964311165E-15,0.));
#17644=DIRECTION('',(0.707106781186548,0.,0.707106781186548));
#17645=DIRECTION('center_axis',(0.,0.,1.));
#17646=DIRECTION('ref_axis',(1.,3.94745964311165E-15,0.));
#17647=DIRECTION('center_axis',(0.,0.,-1.));
#17648=DIRECTION('ref_axis',(1.,3.94745964311165E-15,0.));
#17649=DIRECTION('center_axis',(-0.707106781186548,0.,0.707106781186548));
#17650=DIRECTION('ref_axis',(0.707106781186548,0.,0.707106781186548));
#17651=DIRECTION('',(0.707106781186548,0.,0.707106781186548));
#17652=DIRECTION('',(0.,1.,0.));
#17653=DIRECTION('',(0.,-1.,0.));
#17654=DIRECTION('center_axis',(0.,0.,1.));
#17655=DIRECTION('ref_axis',(9.86864910777915E-16,-1.,0.));
#17656=DIRECTION('center_axis',(0.,0.,1.));
#17657=DIRECTION('ref_axis',(9.86864910777915E-16,-1.,0.));
#17658=DIRECTION('center_axis',(0.,0.,-1.));
#17659=DIRECTION('ref_axis',(9.86864910777915E-16,-1.,0.));
#17660=DIRECTION('center_axis',(0.,0.,1.));
#17661=DIRECTION('ref_axis',(1.,0.,0.));
#17662=DIRECTION('',(0.707106781186541,-0.707106781186554,0.));
#17663=DIRECTION('',(0.,-1.,0.));
#17664=DIRECTION('',(-1.,0.,0.));
#17665=DIRECTION('center_axis',(0.,0.,-1.));
#17666=DIRECTION('ref_axis',(1.26882631385732E-15,-1.,0.));
#17667=DIRECTION('',(0.,-1.,0.));
#17668=DIRECTION('center_axis',(0.,0.,-1.));
#17669=DIRECTION('ref_axis',(1.,1.26882631385732E-15,0.));
#17670=DIRECTION('',(1.,0.,0.));
#17671=DIRECTION('center_axis',(0.,0.,-1.));
#17672=DIRECTION('ref_axis',(-9.51619735392991E-16,1.,0.));
#17673=DIRECTION('',(0.,1.,0.));
#17674=DIRECTION('center_axis',(0.,0.,-1.));
#17675=DIRECTION('ref_axis',(-1.,-1.26882631385732E-15,0.));
#17676=DIRECTION('',(-1.,0.,0.));
#17677=DIRECTION('',(0.,1.,0.));
#17678=DIRECTION('',(0.707106781186543,0.707106781186552,0.));
#17679=DIRECTION('center_axis',(0.,0.,-1.));
#17680=DIRECTION('ref_axis',(-2.46716227694479E-15,1.,0.));
#17681=DIRECTION('',(0.,0.,-1.));
#17682=DIRECTION('center_axis',(0.,0.,-1.));
#17683=DIRECTION('ref_axis',(-2.46716227694479E-15,1.,0.));
#17684=DIRECTION('',(0.,0.,-1.));
#17685=DIRECTION('center_axis',(-1.,0.,0.));
#17686=DIRECTION('ref_axis',(0.,1.,0.));
#17687=DIRECTION('',(0.,0.,-1.));
#17688=DIRECTION('',(0.,1.,0.));
#17689=DIRECTION('center_axis',(0.,0.,-1.));
#17690=DIRECTION('ref_axis',(-1.,-1.97372982155583E-15,0.));
#17691=DIRECTION('',(0.,0.,-1.));
#17692=DIRECTION('center_axis',(0.,0.,-1.));
#17693=DIRECTION('ref_axis',(-1.,-1.97372982155583E-15,0.));
#17694=DIRECTION('center_axis',(0.,-1.,0.));
#17695=DIRECTION('ref_axis',(-1.,0.,0.));
#17696=DIRECTION('',(0.,0.,-1.));
#17697=DIRECTION('',(-1.,0.,0.));
#17698=DIRECTION('center_axis',(0.57735026918963,0.57735026918962,0.577350269189628));
#17699=DIRECTION('ref_axis',(0.707106781186546,0.,-0.707106781186549));
#17700=DIRECTION('',(0.707106781186541,-0.707106781186554,0.));
#17701=DIRECTION('',(0.,0.707106781186552,-0.707106781186543));
#17702=DIRECTION('',(-0.707106781186546,0.,0.707106781186549));
#17703=DIRECTION('center_axis',(0.,0.707106781186543,0.707106781186552));
#17704=DIRECTION('ref_axis',(1.,0.,0.));
#17705=DIRECTION('',(0.577350269189623,-0.577350269189631,0.577350269189623));
#17706=DIRECTION('',(1.,0.,0.));
#17707=DIRECTION('',(-1.,0.,0.));
#17708=DIRECTION('',(-0.577350269189623,-0.577350269189631,0.577350269189623));
#17709=DIRECTION('center_axis',(0.707106781186549,0.,0.707106781186546));
#17710=DIRECTION('ref_axis',(0.707106781186546,0.,-0.707106781186549));
#17711=DIRECTION('',(0.577350269189628,0.577350269189618,-0.577350269189631));
#17712=DIRECTION('',(0.,1.,0.));
#17713=DIRECTION('',(0.,-1.,0.));
#17714=DIRECTION('',(0.577350269189628,-0.577350269189618,-0.577350269189631));
#17715=DIRECTION('center_axis',(0.707106781186554,0.707106781186541,0.));
#17716=DIRECTION('ref_axis',(0.,0.,-1.));
#17717=DIRECTION('',(0.,0.,1.));
#17718=DIRECTION('',(0.,0.,-1.));
#17719=DIRECTION('center_axis',(0.,0.,1.));
#17720=DIRECTION('ref_axis',(-1.,0.,0.));
#17721=DIRECTION('',(0.,1.,0.));
#17722=DIRECTION('',(-1.,0.,0.));
#17723=DIRECTION('center_axis',(-0.707106781186548,0.,0.707106781186548));
#17724=DIRECTION('ref_axis',(0.707106781186548,0.,0.707106781186548));
#17725=DIRECTION('',(0.577350269189623,0.577350269189631,0.577350269189623));
#17726=DIRECTION('',(0.,-1.,0.));
#17727=DIRECTION('',(0.707106781186547,0.,0.707106781186547));
#17728=DIRECTION('center_axis',(-0.707106781186552,0.707106781186543,0.));
#17729=DIRECTION('ref_axis',(0.,0.,1.));
#17730=DIRECTION('',(0.,0.,-1.));
#17731=DIRECTION('',(0.,0.,1.));
#17732=DIRECTION('center_axis',(0.,1.,0.));
#17733=DIRECTION('ref_axis',(1.,0.,0.));
#17734=DIRECTION('',(0.881917103688204,0.,-0.471404520791018));
#17735=DIRECTION('',(0.,0.881917103688206,0.471404520791014));
#17736=DIRECTION('',(0.465319173178999,-0.504527148397124,-0.727276029855432));
#17737=DIRECTION('center_axis',(0.,0.,1.));
#17738=DIRECTION('ref_axis',(-9.5161973539299E-16,1.,0.));
#17739=DIRECTION('',(-0.5050762722761,0.494871659305393,0.707106781186552));
#17740=DIRECTION('center_axis',(0.,0.,-1.));
#17741=DIRECTION('ref_axis',(-9.51619735392991E-16,1.,0.));
#17742=DIRECTION('',(0.49487165930539,-0.505076272276101,-0.707106781186553));
#17743=DIRECTION('center_axis',(0.,0.,1.));
#17744=DIRECTION('ref_axis',(-9.51619735392991E-16,1.,0.));
#17745=DIRECTION('',(-0.504527148397126,0.465319173179001,0.72727602985543));
#17746=DIRECTION('center_axis',(-1.,0.,0.));
#17747=DIRECTION('ref_axis',(0.,0.707106781186546,-0.707106781186549));
#17748=DIRECTION('',(1.,0.,0.));
#17749=DIRECTION('',(-1.,0.,0.));
#17750=DIRECTION('center_axis',(0.,1.,0.));
#17751=DIRECTION('ref_axis',(-1.,0.,0.));
#17752=DIRECTION('',(0.,0.,1.));
#17753=DIRECTION('',(-1.,0.,0.));
#17754=DIRECTION('',(0.,0.,1.));
#17755=DIRECTION('',(0.881917103688202,0.,0.471404520791021));
#17756=DIRECTION('center_axis',(0.,0.,1.));
#17757=DIRECTION('ref_axis',(-9.51619735392991E-16,1.,0.));
#17758=DIRECTION('',(0.,0.,1.));
#17759=DIRECTION('center_axis',(0.,0.,1.));
#17760=DIRECTION('ref_axis',(-9.51619735392991E-16,1.,0.));
#17761=DIRECTION('',(0.,-0.881917103688202,-0.471404520791021));
#17762=DIRECTION('',(-0.504527148397114,-0.465319173179004,-0.727276029855435));
#17763=DIRECTION('center_axis',(0.,0.,1.));
#17764=DIRECTION('ref_axis',(1.,1.26882631385732E-15,0.));
#17765=DIRECTION('',(0.494871659305391,0.505076272276104,0.70710678118655));
#17766=DIRECTION('center_axis',(0.,0.,-1.));
#17767=DIRECTION('ref_axis',(1.,1.26882631385732E-15,0.));
#17768=DIRECTION('',(-0.505076272276111,-0.494871659305385,-0.70710678118655));
#17769=DIRECTION('center_axis',(0.,0.,1.));
#17770=DIRECTION('ref_axis',(1.,1.26882631385732E-15,0.));
#17771=DIRECTION('',(0.465319173178992,0.504527148397119,0.72727602985544));
#17772=DIRECTION('center_axis',(0.,0.,1.));
#17773=DIRECTION('ref_axis',(1.,0.,0.));
#17774=DIRECTION('',(0.,1.,0.));
#17775=DIRECTION('center_axis',(0.,0.,1.));
#17776=DIRECTION('ref_axis',(1.26882631385732E-15,-1.,0.));
#17777=DIRECTION('',(1.,0.,0.));
#17778=DIRECTION('center_axis',(0.,0.,1.));
#17779=DIRECTION('ref_axis',(-1.,-1.26882631385732E-15,0.));
#17780=DIRECTION('',(0.,-1.,0.));
#17781=DIRECTION('center_axis',(-0.577350269189622,-0.577350269189634,0.577350269189622));
#17782=DIRECTION('ref_axis',(0.707106781186547,0.,0.707106781186547));
#17783=DIRECTION('',(0.,-0.70710678118654,-0.707106781186555));
#17784=DIRECTION('',(-0.707106781186555,0.70710678118654,0.));
#17785=DIRECTION('center_axis',(0.,-0.707106781186555,0.70710678118654));
#17786=DIRECTION('ref_axis',(1.,0.,0.));
#17787=DIRECTION('',(1.,0.,0.));
#17788=DIRECTION('',(0.577350269189628,0.577350269189618,0.577350269189631));
#17789=DIRECTION('center_axis',(0.,-0.707106781186548,0.707106781186548));
#17790=DIRECTION('ref_axis',(1.,0.,0.));
#17791=DIRECTION('',(1.,0.,0.));
#17792=DIRECTION('',(0.,0.707106781186548,0.707106781186548));
#17793=DIRECTION('',(-0.577350269189629,-0.577350269189619,-0.577350269189629));
#17794=DIRECTION('center_axis',(0.,0.,-1.));
#17795=DIRECTION('ref_axis',(1.26882631385732E-15,-1.,0.));
#17796=DIRECTION('',(-0.707106781186548,0.,0.707106781186548));
#17797=DIRECTION('center_axis',(0.,0.,1.));
#17798=DIRECTION('ref_axis',(1.26882631385732E-15,-1.,0.));
#17799=DIRECTION('center_axis',(0.707106781186548,0.,0.707106781186548));
#17800=DIRECTION('ref_axis',(0.707106781186548,0.,-0.707106781186548));
#17801=DIRECTION('',(-0.707106781186548,0.,0.707106781186548));
#17802=DIRECTION('',(0.,1.,0.));
#17803=DIRECTION('center_axis',(0.,0.,-1.));
#17804=DIRECTION('ref_axis',(1.,1.26882631385732E-15,0.));
#17805=DIRECTION('',(0.,-0.707106781186548,0.707106781186548));
#17806=DIRECTION('center_axis',(0.,0.,1.));
#17807=DIRECTION('ref_axis',(1.,1.26882631385732E-15,0.));
#17808=DIRECTION('center_axis',(0.,0.707106781186548,0.707106781186548));
#17809=DIRECTION('ref_axis',(1.,0.,0.));
#17810=DIRECTION('',(0.,-0.707106781186548,0.707106781186548));
#17811=DIRECTION('center_axis',(0.,0.,-1.));
#17812=DIRECTION('ref_axis',(-9.5161973539299E-16,1.,0.));
#17813=DIRECTION('',(0.707106781186549,0.,0.707106781186546));
#17814=DIRECTION('center_axis',(-0.707106781186546,0.,0.707106781186549));
#17815=DIRECTION('ref_axis',(0.707106781186549,0.,0.707106781186546));
#17816=DIRECTION('',(0.707106781186549,0.,0.707106781186546));
#17817=DIRECTION('',(0.,-1.,0.));
#17818=DIRECTION('center_axis',(0.,0.,-1.));
#17819=DIRECTION('ref_axis',(-1.,-1.26882631385732E-15,0.));
#17820=DIRECTION('',(0.,0.707106781186548,0.707106781186548));
#17821=DIRECTION('center_axis',(0.,0.,1.));
#17822=DIRECTION('ref_axis',(-1.,-1.26882631385732E-15,0.));
#17823=DIRECTION('center_axis',(0.,-0.707106781186548,0.707106781186548));
#17824=DIRECTION('ref_axis',(1.,0.,0.));
#17825=DIRECTION('',(1.,0.,0.));
#17826=DIRECTION('',(-0.577350269189632,0.577350269189618,0.577350269189628));
#17827=DIRECTION('center_axis',(0.707106781186541,-0.707106781186554,0.));
#17828=DIRECTION('ref_axis',(0.,0.,-1.));
#17829=DIRECTION('',(0.,0.,-1.));
#17830=DIRECTION('',(0.,0.,1.));
#17831=DIRECTION('center_axis',(-0.70710678118654,-0.707106781186555,0.));
#17832=DIRECTION('ref_axis',(0.,0.,1.));
#17833=DIRECTION('',(0.,0.,1.));
#17834=DIRECTION('',(0.,0.,-1.));
#17835=DIRECTION('center_axis',(0.,0.,1.));
#17836=DIRECTION('ref_axis',(1.,1.26882631385732E-15,0.));
#17837=DIRECTION('',(0.,0.,1.));
#17838=DIRECTION('center_axis',(1.,0.,0.));
#17839=DIRECTION('ref_axis',(0.,1.,0.));
#17840=DIRECTION('',(0.,0.,1.));
#17841=DIRECTION('',(0.,-0.881917103688205,0.471404520791017));
#17842=DIRECTION('',(0.,-1.,0.));
#17843=DIRECTION('center_axis',(0.,0.,1.));
#17844=DIRECTION('ref_axis',(1.26882631385732E-15,-1.,0.));
#17845=DIRECTION('',(0.,0.,1.));
#17846=DIRECTION('center_axis',(0.,0.,-1.));
#17847=DIRECTION('ref_axis',(1.26882631385732E-15,-1.,0.));
#17848=DIRECTION('center_axis',(-1.,0.,0.));
#17849=DIRECTION('ref_axis',(0.,0.,-1.));
#17850=DIRECTION('center_axis',(1.,0.,0.));
#17851=DIRECTION('ref_axis',(0.,0.,1.));
#17852=DIRECTION('',(0.,0.881917103688198,-0.471404520791029));
#17853=DIRECTION('',(-0.881917103688201,0.,0.471404520791024));
#17854=DIRECTION('',(0.504527148397123,0.46531917317901,-0.727276029855426));
#17855=DIRECTION('center_axis',(0.,0.,1.));
#17856=DIRECTION('ref_axis',(-1.,-1.26882631385732E-15,0.));
#17857=DIRECTION('',(-0.49487165930539,-0.505076272276101,0.707106781186553));
#17858=DIRECTION('center_axis',(0.,0.,-1.));
#17859=DIRECTION('ref_axis',(-1.,-1.26882631385732E-15,0.));
#17860=DIRECTION('',(0.505076272276103,0.494871659305383,-0.707106781186557));
#17861=DIRECTION('',(-0.465319173178996,-0.504527148397133,0.727276029855427));
#17862=DIRECTION('center_axis',(0.,-1.,0.));
#17863=DIRECTION('ref_axis',(-0.707106781186546,0.,-0.707106781186549));
#17864=DIRECTION('',(0.,1.,0.));
#17865=DIRECTION('center_axis',(-1.,0.,0.));
#17866=DIRECTION('ref_axis',(0.,-1.,0.));
#17867=DIRECTION('',(0.,0.,1.));
#17868=DIRECTION('center_axis',(0.,0.,1.));
#17869=DIRECTION('ref_axis',(-1.,-1.26882631385732E-15,0.));
#17870=DIRECTION('',(0.,0.,1.));
#17871=DIRECTION('',(-0.881917103688201,0.,-0.471404520791023));
#17872=DIRECTION('',(-0.465319173178989,0.504527148397135,-0.727276029855431));
#17873=DIRECTION('center_axis',(0.,0.,1.));
#17874=DIRECTION('ref_axis',(1.26882631385732E-15,-1.,0.));
#17875=DIRECTION('',(0.5050762722761,-0.494871659305393,0.707106781186552));
#17876=DIRECTION('',(-0.494871659305393,0.5050762722761,-0.707106781186552));
#17877=DIRECTION('',(0.50452714839712,-0.465319173179011,0.727276029855427));
#17878=DIRECTION('center_axis',(0.,1.,0.));
#17879=DIRECTION('ref_axis',(0.707106781186548,0.,-0.707106781186548));
#17880=DIRECTION('center_axis',(1.,0.,0.));
#17881=DIRECTION('ref_axis',(0.,-0.707106781186548,-0.707106781186548));
#17882=DIRECTION('',(-1.,0.,0.));
#17883=DIRECTION('center_axis',(0.,-1.,0.));
#17884=DIRECTION('ref_axis',(1.,0.,0.));
#17885=DIRECTION('center_axis',(0.,0.,-1.));
#17886=DIRECTION('ref_axis',(9.86864910777915E-16,-1.,0.));
#17887=DIRECTION('',(0.,0.,-1.));
#17888=DIRECTION('center_axis',(0.,0.,-1.));
#17889=DIRECTION('ref_axis',(9.86864910777915E-16,-1.,0.));
#17890=DIRECTION('center_axis',(1.,0.,0.));
#17891=DIRECTION('ref_axis',(0.,-1.,0.));
#17892=DIRECTION('',(0.,0.,-1.));
#17893=DIRECTION('',(0.,-1.,0.));
#17894=DIRECTION('center_axis',(0.,0.,-1.));
#17895=DIRECTION('ref_axis',(1.,3.94745964311165E-15,0.));
#17896=DIRECTION('',(0.,0.,-1.));
#17897=DIRECTION('center_axis',(0.,0.,-1.));
#17898=DIRECTION('ref_axis',(1.,3.94745964311165E-15,0.));
#17899=DIRECTION('center_axis',(0.,1.,0.));
#17900=DIRECTION('ref_axis',(1.,0.,0.));
#17901=DIRECTION('',(1.,0.,0.));
#17902=DIRECTION('center_axis',(0.,0.,1.));
#17903=DIRECTION('ref_axis',(1.,0.,0.));
#17904=DIRECTION('axis',(0.,0.,1.));
#17905=DIRECTION('refdir',(1.,0.,0.));
#17906=DIRECTION('center_axis',(-1.,0.,0.));
#17907=DIRECTION('ref_axis',(0.,0.,-1.));
#17908=DIRECTION('center_axis',(1.,0.,0.));
#17909=DIRECTION('ref_axis',(0.,0.,-1.));
#17910=DIRECTION('',(-0.707106781186548,-8.65956056235493E-17,0.707106781186547));
#17911=DIRECTION('center_axis',(-1.,0.,0.));
#17912=DIRECTION('ref_axis',(0.,0.,-1.));
#17913=DIRECTION('center_axis',(1.,0.,0.));
#17914=DIRECTION('ref_axis',(0.,0.,-1.));
#17915=DIRECTION('center_axis',(-1.,0.,0.));
#17916=DIRECTION('ref_axis',(0.,0.,-1.));
#17917=DIRECTION('',(-1.,0.,0.));
#17918=DIRECTION('center_axis',(1.,0.,0.));
#17919=DIRECTION('ref_axis',(0.,0.,-1.));
#17920=DIRECTION('',(0.,-0.309016994374948,0.951056516295153));
#17921=DIRECTION('',(0.,0.309016994374948,0.951056516295153));
#17922=DIRECTION('',(0.,0.809016994374947,0.587785252292473));
#17923=DIRECTION('',(0.,1.,-2.24547323617027E-16));
#17924=DIRECTION('',(0.,0.809016994374947,-0.587785252292473));
#17925=DIRECTION('',(0.,0.309016994374948,-0.951056516295153));
#17926=DIRECTION('',(0.,-0.309016994374948,-0.951056516295153));
#17927=DIRECTION('',(0.,-0.809016994374947,-0.587785252292473));
#17928=DIRECTION('',(0.,-1.,2.24547323617027E-16));
#17929=DIRECTION('',(0.,-0.809016994374947,0.587785252292473));
#17930=DIRECTION('center_axis',(1.,0.,0.));
#17931=DIRECTION('ref_axis',(0.,0.,-1.));
#17932=DIRECTION('center_axis',(1.,0.,0.));
#17933=DIRECTION('ref_axis',(0.,0.,-1.));
#17934=DIRECTION('',(-0.707106781186548,8.65956056235493E-17,-0.707106781186547));
#17935=DIRECTION('center_axis',(1.,0.,0.));
#17936=DIRECTION('ref_axis',(0.,0.,-1.));
#17937=DIRECTION('',(0.,0.951056516295154,0.309016994374947));
#17938=DIRECTION('',(0.,-0.309016994374948,0.951056516295154));
#17939=DIRECTION('',(0.,0.587785252292475,-0.809016994374946));
#17940=DIRECTION('',(0.,-0.809016994374947,0.587785252292473));
#17941=DIRECTION('',(0.,-0.587785252292473,-0.809016994374947));
#17942=DIRECTION('',(0.,0.809016994374947,-0.587785252292473));
#17943=DIRECTION('',(0.,0.587785252292473,0.809016994374947));
#17944=DIRECTION('',(0.,-0.809016994374947,0.587785252292473));
#17945=DIRECTION('',(0.,0.951056516295153,-0.30901699437495));
#17946=DIRECTION('',(0.,-1.,2.24547323617027E-16));
#17947=DIRECTION('',(0.,-5.55111512312578E-17,-1.));
#17948=DIRECTION('',(0.,1.,1.66533453693773E-16));
#17949=DIRECTION('',(0.,3.33066907387547E-16,1.));
#17950=DIRECTION('',(0.,-1.,2.24547323617027E-16));
#17951=DIRECTION('',(0.,0.951056516295154,0.309016994374946));
#17952=DIRECTION('',(0.,-0.809016994374947,-0.587785252292473));
#17953=DIRECTION('',(0.,0.587785252292473,-0.809016994374947));
#17954=DIRECTION('',(0.,0.809016994374947,0.587785252292473));
#17955=DIRECTION('',(0.,-0.587785252292473,0.809016994374948));
#17956=DIRECTION('',(0.,-0.809016994374947,-0.587785252292473));
#17957=DIRECTION('',(0.,0.587785252292478,0.809016994374944));
#17958=DIRECTION('',(0.,-0.309016994374948,-0.951056516295153));
#17959=DIRECTION('',(0.,0.951056516295153,-0.309016994374948));
#17960=DIRECTION('',(0.,0.309016994374947,0.951056516295154));
#17961=DIRECTION('',(0.,-0.951056516295153,0.309016994374948));
#17962=DIRECTION('',(0.,-0.309016994374948,-0.951056516295153));
#17963=DIRECTION('',(0.,0.,1.));
#17964=DIRECTION('',(0.,0.309016994374948,-0.951056516295153));
#17965=DIRECTION('',(0.,0.951056516295154,0.309016994374947));
#17966=DIRECTION('',(0.,-0.309016994374948,0.951056516295153));
#17967=DIRECTION('',(0.,-0.951056516295154,-0.309016994374947));
#17968=DIRECTION('',(0.,0.309016994374948,-0.951056516295154));
#17969=DIRECTION('',(0.,-0.587785252292475,0.809016994374946));
#17970=DIRECTION('',(0.,0.809016994374947,-0.587785252292473));
#17971=DIRECTION('',(0.,0.587785252292473,0.809016994374947));
#17972=DIRECTION('',(0.,-0.809016994374947,0.587785252292473));
#17973=DIRECTION('',(0.,-0.587785252292473,-0.809016994374947));
#17974=DIRECTION('',(0.,0.809016994374947,-0.587785252292473));
#17975=DIRECTION('',(0.,-0.951056516295154,0.309016994374947));
#17976=DIRECTION('',(0.,1.,-2.24547323617027E-16));
#17977=DIRECTION('',(0.,1.66533453693773E-16,1.));
#17978=DIRECTION('',(0.,-1.,-5.55111512312578E-17));
#17979=DIRECTION('',(0.,-4.44089209850063E-16,-1.));
#17980=DIRECTION('',(0.,1.,-2.24547323617027E-16));
#17981=DIRECTION('',(0.,-0.951056516295153,-0.309016994374949));
#17982=DIRECTION('',(0.,0.809016994374947,0.587785252292473));
#17983=DIRECTION('',(0.,-0.587785252292473,0.809016994374947));
#17984=DIRECTION('',(0.,-0.809016994374947,-0.587785252292473));
#17985=DIRECTION('',(0.,0.587785252292473,-0.809016994374948));
#17986=DIRECTION('',(0.,0.809016994374948,0.587785252292473));
#17987=DIRECTION('',(0.,-0.587785252292472,-0.809016994374948));
#17988=DIRECTION('',(0.,0.309016994374948,0.951056516295153));
#17989=DIRECTION('',(0.,-0.951056516295153,0.309016994374948));
#17990=DIRECTION('',(0.,-0.309016994374948,-0.951056516295154));
#17991=DIRECTION('',(0.,0.951056516295153,-0.309016994374948));
#17992=DIRECTION('',(0.,0.309016994374948,0.951056516295153));
#17993=DIRECTION('',(0.,0.,-1.));
#17994=DIRECTION('',(0.,-0.309016994374948,0.951056516295153));
#17995=DIRECTION('',(0.,-0.951056516295154,-0.309016994374947));
#17996=DIRECTION('',(0.,0.309016994374948,-0.951056516295153));
#17997=DIRECTION('center_axis',(0.707106781186548,0.672498511963957,0.218508012224411));
#17998=DIRECTION('ref_axis',(0.295241808844326,0.,-0.955422563220238));
#17999=DIRECTION('',(0.707106781186547,-0.672498511963958,-0.218508012224411));
#18000=DIRECTION('',(0.,-0.309016994374948,0.951056516295153));
#18001=DIRECTION('',(-0.707106781186547,0.672498511963958,0.218508012224411));
#18002=DIRECTION('center_axis',(0.,-0.951056516295154,-0.309016994374948));
#18003=DIRECTION('ref_axis',(0.,0.309016994374948,-0.951056516295153));
#18004=DIRECTION('',(1.,0.,0.));
#18005=DIRECTION('',(0.,-0.309016994374948,0.951056516295153));
#18006=DIRECTION('',(1.,0.,0.));
#18007=DIRECTION('center_axis',(0.707106781186547,0.415626937777453,0.572061402817685));
#18008=DIRECTION('ref_axis',(0.628960169645094,0.,-0.777437524821136));
#18009=DIRECTION('',(0.707106781186548,-0.415626937777453,-0.572061402817684));
#18010=DIRECTION('',(0.,-0.809016994374947,0.587785252292473));
#18011=DIRECTION('',(-0.707106781186548,0.415626937777453,0.572061402817684));
#18012=DIRECTION('center_axis',(0.,-0.587785252292473,-0.809016994374948));
#18013=DIRECTION('ref_axis',(0.,0.809016994374947,-0.587785252292473));
#18014=DIRECTION('',(1.,0.,0.));
#18015=DIRECTION('',(0.,-0.809016994374947,0.587785252292473));
#18016=DIRECTION('',(1.,0.,0.));
#18017=DIRECTION('center_axis',(0.707106781186548,-1.17756934401283E-16,
0.707106781186548));
#18018=DIRECTION('ref_axis',(0.707106781186548,0.,-0.707106781186548));
#18019=DIRECTION('',(0.707106781186548,-3.92523114670944E-17,-0.707106781186548));
#18020=DIRECTION('',(0.,-1.,-1.66533453693773E-16));
#18021=DIRECTION('',(-0.707106781186548,2.35513868802566E-16,0.707106781186548));
#18022=DIRECTION('center_axis',(0.,1.66533453693773E-16,-1.));
#18023=DIRECTION('ref_axis',(0.,1.,1.66533453693773E-16));
#18024=DIRECTION('',(1.,0.,0.));
#18025=DIRECTION('',(0.,-1.,-1.66533453693773E-16));
#18026=DIRECTION('',(1.,0.,0.));
#18027=DIRECTION('center_axis',(-0.596110861367214,0.649561473330963,0.471934034928767));
#18028=DIRECTION('ref_axis',(0.620713403652074,0.,0.784037544079783));
#18029=DIRECTION('',(0.,-0.587785252292475,0.809016994374946));
#18030=DIRECTION('',(0.638130334584325,0.740019202960846,-0.212511776926577));
#18031=DIRECTION('',(-0.638130334584329,-0.0265677996432243,-0.769469835734585));
#18032=DIRECTION('center_axis',(-0.707106781186548,0.672498511963956,0.21850801222441));
#18033=DIRECTION('ref_axis',(0.295241808844326,0.,0.955422563220239));
#18034=DIRECTION('',(-0.689151757774652,-0.724617040067447,-5.98775806539528E-15));
#18035=DIRECTION('',(0.,0.309016994374948,-0.951056516295153));
#18036=DIRECTION('',(-0.295241808844326,0.,-0.955422563220239));
#18037=DIRECTION('center_axis',(-0.596110861367212,0.248110405029972,0.763605308962624));
#18038=DIRECTION('ref_axis',(0.788252578093854,0.,0.615351828735718));
#18039=DIRECTION('',(0.,-0.951056516295153,0.30901699437495));
#18040=DIRECTION('',(0.638130334584327,0.723599399775037,0.263046734875194));
#18041=DIRECTION('',(-0.63813033458433,0.430789220114182,-0.638130334584327));
#18042=DIRECTION('center_axis',(-0.707106781186546,0.415626937777454,0.572061402817685));
#18043=DIRECTION('ref_axis',(0.628960169645095,0.,0.777437524821135));
#18044=DIRECTION('',(0.,0.809016994374947,-0.587785252292473));
#18045=DIRECTION('center_axis',(-0.596110861367212,-0.24811040502997,0.763605308962624));
#18046=DIRECTION('ref_axis',(0.788252578093855,0.,0.615351828735717));
#18047=DIRECTION('',(0.,-0.951056516295154,-0.309016994374946));
#18048=DIRECTION('',(0.638130334584328,0.430789220114187,0.638130334584326));
#18049=DIRECTION('',(-0.638130334584328,0.723599399775035,-0.263046734875197));
#18050=DIRECTION('center_axis',(-0.707106781186546,1.5877893522689E-16,
0.707106781186549));
#18051=DIRECTION('ref_axis',(0.707106781186549,0.,0.707106781186546));
#18052=DIRECTION('',(0.,1.,-2.24547323617027E-16));
#18053=DIRECTION('center_axis',(-0.707106781186546,-0.415626937777454,0.572061402817685));
#18054=DIRECTION('ref_axis',(0.628960169645095,0.,0.777437524821135));
#18055=DIRECTION('',(0.295241808844322,0.561583292368335,0.772953090454443));
#18056=DIRECTION('',(0.,0.809016994374947,0.587785252292473));
#18057=DIRECTION('',(0.689151757774653,-0.586227499828236,0.425919209711468));
#18058=DIRECTION('center_axis',(0.,-0.309016994374946,0.951056516295154));
#18059=DIRECTION('ref_axis',(1.,0.,0.));
#18060=DIRECTION('',(-1.,0.,0.));
#18061=DIRECTION('',(1.,0.,0.));
#18062=DIRECTION('center_axis',(0.,0.30901699437495,0.951056516295153));
#18063=DIRECTION('ref_axis',(1.,0.,0.));
#18064=DIRECTION('',(-1.,0.,0.));
#18065=DIRECTION('',(1.,0.,0.));
#18066=DIRECTION('center_axis',(0.,0.809016994374946,0.587785252292475));
#18067=DIRECTION('ref_axis',(1.,0.,0.));
#18068=DIRECTION('',(-1.,0.,0.));
#18069=DIRECTION('',(1.,0.,0.));
#18070=DIRECTION('center_axis',(0.,0.587785252292473,0.809016994374947));
#18071=DIRECTION('ref_axis',(0.,-0.809016994374947,0.587785252292473));
#18072=DIRECTION('',(-1.,0.,0.));
#18073=DIRECTION('',(0.,0.809016994374947,-0.587785252292473));
#18074=DIRECTION('',(1.,0.,0.));
#18075=DIRECTION('center_axis',(0.,2.24547323617027E-16,1.));
#18076=DIRECTION('ref_axis',(0.,-1.,2.24547323617027E-16));
#18077=DIRECTION('',(-1.,0.,0.));
#18078=DIRECTION('',(0.,1.,-2.24547323617027E-16));
#18079=DIRECTION('',(1.,0.,0.));
#18080=DIRECTION('center_axis',(0.,-0.587785252292473,0.809016994374947));
#18081=DIRECTION('ref_axis',(0.,-0.809016994374947,-0.587785252292473));
#18082=DIRECTION('',(-1.,0.,0.));
#18083=DIRECTION('',(-1.,0.,0.));
#18084=DIRECTION('',(0.,0.809016994374947,0.587785252292473));
#18085=DIRECTION('',(1.,0.,0.));
#18086=DIRECTION('center_axis',(0.,-0.809016994374944,0.587785252292478));
#18087=DIRECTION('ref_axis',(1.,0.,0.));
#18088=DIRECTION('',(-0.295241808844332,0.561583292368333,0.77295309045444));
#18089=DIRECTION('',(1.,0.,0.));
#18090=DIRECTION('center_axis',(-0.707106781186547,-0.672498511963958,0.218508012224411));
#18091=DIRECTION('ref_axis',(0.295241808844327,0.,0.955422563220238));
#18092=DIRECTION('',(0.638130334584329,-0.473776822943218,0.60689801295203));
#18093=DIRECTION('',(0.,0.309016994374948,0.951056516295153));
#18094=DIRECTION('center_axis',(0.707106781186548,-0.415626937777453,0.572061402817684));
#18095=DIRECTION('ref_axis',(0.628960169645094,0.,-0.777437524821136));
#18096=DIRECTION('',(0.707106781186547,0.415626937777454,-0.572061402817685));
#18097=DIRECTION('',(0.,-0.809016994374947,-0.587785252292473));
#18098=DIRECTION('',(-0.707106781186547,-0.415626937777453,0.572061402817685));
#18099=DIRECTION('center_axis',(0.,0.587785252292473,-0.809016994374947));
#18100=DIRECTION('ref_axis',(0.,0.809016994374947,0.587785252292473));
#18101=DIRECTION('',(1.,0.,0.));
#18102=DIRECTION('',(0.,-0.809016994374947,-0.587785252292473));
#18103=DIRECTION('',(1.,0.,0.));
#18104=DIRECTION('center_axis',(0.707106781186546,-0.672498511963958,0.218508012224411));
#18105=DIRECTION('ref_axis',(0.295241808844327,0.,-0.955422563220238));
#18106=DIRECTION('',(0.707106781186549,0.672498511963956,-0.21850801222441));
#18107=DIRECTION('',(0.,-0.309016994374947,-0.951056516295154));
#18108=DIRECTION('',(-0.707106781186549,-0.672498511963956,0.21850801222441));
#18109=DIRECTION('center_axis',(0.,0.951056516295154,-0.309016994374947));
#18110=DIRECTION('ref_axis',(0.,0.309016994374947,0.951056516295154));
#18111=DIRECTION('',(1.,0.,0.));
#18112=DIRECTION('',(0.,-0.309016994374947,-0.951056516295154));
#18113=DIRECTION('',(1.,0.,0.));
#18114=DIRECTION('center_axis',(0.707106781186546,-0.672498511963958,-0.218508012224411));
#18115=DIRECTION('ref_axis',(-0.295241808844327,0.,-0.955422563220238));
#18116=DIRECTION('',(0.707106781186549,0.672498511963956,0.21850801222441));
#18117=DIRECTION('',(0.,0.309016994374948,-0.951056516295153));
#18118=DIRECTION('',(-0.707106781186549,-0.672498511963956,-0.21850801222441));
#18119=DIRECTION('center_axis',(0.,0.951056516295154,0.309016994374948));
#18120=DIRECTION('ref_axis',(0.,-0.309016994374948,0.951056516295153));
#18121=DIRECTION('',(1.,0.,0.));
#18122=DIRECTION('',(0.,0.309016994374948,-0.951056516295153));
#18123=DIRECTION('',(1.,0.,0.));
#18124=DIRECTION('center_axis',(0.707106781186545,-0.415626937777455,-0.572061402817686));
#18125=DIRECTION('ref_axis',(-0.628960169645096,0.,-0.777437524821134));
#18126=DIRECTION('',(0.70710678118655,0.415626937777452,0.572061402817683));
#18127=DIRECTION('',(0.,0.809016994374947,-0.587785252292473));
#18128=DIRECTION('',(-0.70710678118655,-0.415626937777452,-0.572061402817682));
#18129=DIRECTION('center_axis',(0.,0.587785252292473,0.809016994374948));
#18130=DIRECTION('ref_axis',(0.,-0.809016994374947,0.587785252292473));
#18131=DIRECTION('',(1.,0.,0.));
#18132=DIRECTION('',(0.,0.809016994374947,-0.587785252292473));
#18133=DIRECTION('',(1.,0.,0.));
#18134=DIRECTION('center_axis',(0.707106781186548,3.92523114670944E-17,
-0.707106781186548));
#18135=DIRECTION('ref_axis',(-0.707106781186548,0.,-0.707106781186548));
#18136=DIRECTION('',(0.707106781186548,1.17756934401283E-16,0.707106781186548));
#18137=DIRECTION('',(0.,1.,5.55111512312578E-17));
#18138=DIRECTION('',(-0.707106781186548,-3.14018491736755E-16,-0.707106781186548));
#18139=DIRECTION('center_axis',(0.,-5.55111512312578E-17,1.));
#18140=DIRECTION('ref_axis',(0.,-1.,-5.55111512312578E-17));
#18141=DIRECTION('',(1.,0.,0.));
#18142=DIRECTION('',(0.,1.,5.55111512312578E-17));
#18143=DIRECTION('',(1.,0.,0.));
#18144=DIRECTION('center_axis',(0.707106781186548,0.415626937777453,-0.572061402817684));
#18145=DIRECTION('ref_axis',(-0.628960169645094,0.,-0.777437524821136));
#18146=DIRECTION('',(0.707106781186547,-0.415626937777454,0.572061402817685));
#18147=DIRECTION('',(0.,0.809016994374947,0.587785252292473));
#18148=DIRECTION('',(-0.707106781186547,0.415626937777453,-0.572061402817685));
#18149=DIRECTION('center_axis',(0.,-0.587785252292473,0.809016994374947));
#18150=DIRECTION('ref_axis',(0.,-0.809016994374947,-0.587785252292473));
#18151=DIRECTION('',(1.,0.,0.));
#18152=DIRECTION('',(0.,0.809016994374947,0.587785252292473));
#18153=DIRECTION('',(1.,0.,0.));
#18154=DIRECTION('center_axis',(-0.596110861367213,-0.80290213660199,0.));
#18155=DIRECTION('ref_axis',(0.,0.,1.));
#18156=DIRECTION('',(0.,0.,-1.));
#18157=DIRECTION('',(-0.638130334584328,0.473776822943217,0.606898012952033));
#18158=DIRECTION('center_axis',(-0.596110861367212,-0.649561473330965,-0.471934034928767));
#18159=DIRECTION('ref_axis',(-0.620713403652076,0.,0.784037544079782));
#18160=DIRECTION('',(0.,0.587785252292475,-0.809016994374946));
#18161=DIRECTION('',(0.638130334584328,-0.740019202960844,0.212511776926575));
#18162=DIRECTION('',(-0.638130334584327,0.0265677996432183,0.769469835734587));
#18163=DIRECTION('center_axis',(-0.707106781186547,-0.672498511963958,-0.218508012224411));
#18164=DIRECTION('ref_axis',(-0.295241808844327,0.,0.955422563220238));
#18165=DIRECTION('',(0.,-0.309016994374948,0.951056516295153));
#18166=DIRECTION('center_axis',(-0.596110861367213,-0.248110405029968,-0.763605308962624));
#18167=DIRECTION('ref_axis',(-0.788252578093854,0.,0.615351828735718));
#18168=DIRECTION('',(0.,0.951056516295154,-0.309016994374947));
#18169=DIRECTION('',(0.638130334584328,-0.723599399775034,-0.2630467348752));
#18170=DIRECTION('',(-0.638130334584328,-0.430789220114189,0.638130334584325));
#18171=DIRECTION('center_axis',(-0.707106781186546,-0.415626937777454,-0.572061402817685));
#18172=DIRECTION('ref_axis',(-0.628960169645095,0.,0.777437524821135));
#18173=DIRECTION('',(0.,-0.809016994374947,0.587785252292473));
#18174=DIRECTION('center_axis',(-0.596110861367212,0.248110405029972,-0.763605308962624));
#18175=DIRECTION('ref_axis',(-0.788252578093855,0.,0.615351828735717));
#18176=DIRECTION('',(0.,0.951056516295153,0.309016994374949));
#18177=DIRECTION('',(0.638130334584329,-0.430789220114185,-0.638130334584327));
#18178=DIRECTION('',(-0.638130334584327,-0.723599399775037,0.263046734875194));
#18179=DIRECTION('center_axis',(-0.707106781186546,-1.5877893522689E-16,
-0.707106781186549));
#18180=DIRECTION('ref_axis',(-0.707106781186549,0.,0.707106781186546));
#18181=DIRECTION('',(0.,-1.,2.24547323617027E-16));
#18182=DIRECTION('center_axis',(-0.596110861367213,0.649561473330965,-0.471934034928765));
#18183=DIRECTION('ref_axis',(-0.620713403652073,0.,0.784037544079784));
#18184=DIRECTION('',(0.638130334584328,0.0265677996432242,-0.769469835734586));
#18185=DIRECTION('',(-0.638130334584328,-0.740019202960844,-0.212511776926575));
#18186=DIRECTION('',(0.,0.587785252292472,0.809016994374948));
#18187=DIRECTION('center_axis',(-0.707106781186547,0.672498511963958,-0.218508012224411));
#18188=DIRECTION('ref_axis',(-0.295241808844327,0.,0.955422563220238));
#18189=DIRECTION('',(0.295241808844329,0.,-0.955422563220238));
#18190=DIRECTION('',(0.,-0.309016994374948,-0.951056516295153));
#18191=DIRECTION('center_axis',(0.,0.809016994374948,-0.587785252292472));
#18192=DIRECTION('ref_axis',(-1.,0.,0.));
#18193=DIRECTION('',(-1.,0.,0.));
#18194=DIRECTION('',(1.,0.,0.));
#18195=DIRECTION('center_axis',(-0.707106781186546,0.415626937777454,-0.572061402817685));
#18196=DIRECTION('ref_axis',(-0.628960169645095,0.,0.777437524821135));
#18197=DIRECTION('',(0.,-0.809016994374947,-0.587785252292473));
#18198=DIRECTION('center_axis',(0.,1.,0.));
#18199=DIRECTION('ref_axis',(0.,0.,1.));
#18200=DIRECTION('',(1.,0.,0.));
#18201=DIRECTION('',(-1.,0.,0.));
#18202=DIRECTION('center_axis',(0.,0.309016994374949,-0.951056516295153));
#18203=DIRECTION('ref_axis',(-1.,0.,0.));
#18204=DIRECTION('',(-1.,0.,0.));
#18205=DIRECTION('',(1.,0.,0.));
#18206=DIRECTION('center_axis',(0.,-0.309016994374947,-0.951056516295154));
#18207=DIRECTION('ref_axis',(-1.,0.,0.));
#18208=DIRECTION('',(-1.,0.,0.));
#18209=DIRECTION('',(1.,0.,0.));
#18210=DIRECTION('center_axis',(0.,-0.809016994374946,-0.587785252292475));
#18211=DIRECTION('ref_axis',(-1.,0.,0.));
#18212=DIRECTION('',(-1.,0.,0.));
#18213=DIRECTION('',(1.,0.,0.));
#18214=DIRECTION('center_axis',(0.,-1.,0.));
#18215=DIRECTION('ref_axis',(0.,0.,-1.));
#18216=DIRECTION('',(-1.,0.,0.));
#18217=DIRECTION('',(1.,0.,0.));
#18218=DIRECTION('center_axis',(0.,-0.951056516295154,0.309016994374948));
#18219=DIRECTION('ref_axis',(0.,-0.309016994374948,-0.951056516295153));
#18220=DIRECTION('',(-1.,0.,0.));
#18221=DIRECTION('',(0.,0.309016994374948,0.951056516295153));
#18222=DIRECTION('',(1.,0.,0.));
#18223=DIRECTION('center_axis',(0.,-0.951056516295154,-0.309016994374948));
#18224=DIRECTION('ref_axis',(0.,0.309016994374948,-0.951056516295153));
#18225=DIRECTION('',(-1.,0.,0.));
#18226=DIRECTION('',(0.,-0.309016994374948,0.951056516295153));
#18227=DIRECTION('',(1.,0.,0.));
#18228=DIRECTION('center_axis',(0.,-0.587785252292473,-0.809016994374947));
#18229=DIRECTION('ref_axis',(0.,0.809016994374947,-0.587785252292473));
#18230=DIRECTION('',(-1.,0.,0.));
#18231=DIRECTION('',(0.,-0.809016994374947,0.587785252292473));
#18232=DIRECTION('',(1.,0.,0.));
#18233=DIRECTION('center_axis',(0.,-2.24547323617027E-16,-1.));
#18234=DIRECTION('ref_axis',(0.,1.,-2.24547323617027E-16));
#18235=DIRECTION('',(-1.,0.,0.));
#18236=DIRECTION('',(0.,-1.,2.24547323617027E-16));
#18237=DIRECTION('',(1.,0.,0.));
#18238=DIRECTION('center_axis',(0.,0.587785252292473,-0.809016994374948));
#18239=DIRECTION('ref_axis',(0.,0.809016994374947,0.587785252292473));
#18240=DIRECTION('',(-1.,0.,0.));
#18241=DIRECTION('',(0.,-0.809016994374947,-0.587785252292473));
#18242=DIRECTION('',(1.,0.,0.));
#18243=DIRECTION('center_axis',(0.707106781186546,0.672498511963958,-0.218508012224411));
#18244=DIRECTION('ref_axis',(-0.295241808844327,0.,-0.955422563220238));
#18245=DIRECTION('',(0.707106781186549,-0.672498511963956,0.21850801222441));
#18246=DIRECTION('',(0.,0.309016994374948,0.951056516295154));
#18247=DIRECTION('',(-0.707106781186549,0.672498511963956,-0.218508012224411));
#18248=DIRECTION('center_axis',(0.,-0.951056516295154,0.309016994374948));
#18249=DIRECTION('ref_axis',(0.,-0.309016994374948,-0.951056516295154));
#18250=DIRECTION('',(1.,0.,0.));
#18251=DIRECTION('',(0.,0.309016994374948,0.951056516295154));
#18252=DIRECTION('',(1.,0.,0.));
#18253=DIRECTION('center_axis',(1.,0.,0.));
#18254=DIRECTION('ref_axis',(0.,-0.587785252292473,-0.809016994374947));
#18255=DIRECTION('',(0.,-0.309016994374948,-0.951056516295153));
#18256=DIRECTION('',(0.,0.951056516295153,-0.309016994374948));
#18257=DIRECTION('',(0.,-0.951056516295153,0.309016994374948));
#18258=DIRECTION('center_axis',(0.,-0.309016994374948,-0.951056516295154));
#18259=DIRECTION('ref_axis',(0.,0.951056516295153,-0.309016994374948));
#18260=DIRECTION('',(1.,0.,0.));
#18261=DIRECTION('center_axis',(0.,0.309016994374948,0.951056516295153));
#18262=DIRECTION('ref_axis',(0.,-0.951056516295153,0.309016994374948));
#18263=DIRECTION('',(-1.,0.,0.));
#18264=DIRECTION('center_axis',(0.,0.951056516295154,-0.309016994374948));
#18265=DIRECTION('ref_axis',(0.,0.309016994374948,0.951056516295153));
#18266=DIRECTION('center_axis',(1.,0.,0.));
#18267=DIRECTION('ref_axis',(0.,-0.951056516295154,-0.309016994374947));
#18268=DIRECTION('',(0.,0.587785252292473,-0.809016994374948));
#18269=DIRECTION('',(0.,-0.587785252292473,0.809016994374947));
#18270=DIRECTION('center_axis',(0.,-0.809016994374948,-0.587785252292473));
#18271=DIRECTION('ref_axis',(0.,0.587785252292473,-0.809016994374947));
#18272=DIRECTION('center_axis',(0.,0.809016994374948,0.587785252292473));
#18273=DIRECTION('ref_axis',(0.,-0.587785252292473,0.809016994374948));
#18274=DIRECTION('center_axis',(1.,0.,0.));
#18275=DIRECTION('ref_axis',(0.,-0.951056516295153,0.309016994374948));
#18276=DIRECTION('',(0.,-4.44089209850063E-16,-1.));
#18277=DIRECTION('',(0.,1.66533453693773E-16,1.));
#18278=DIRECTION('center_axis',(0.,-1.,1.66533453693773E-16));
#18279=DIRECTION('ref_axis',(0.,-1.66533453693773E-16,-1.));
#18280=DIRECTION('center_axis',(0.,1.,-4.44089209850063E-16));
#18281=DIRECTION('ref_axis',(0.,4.44089209850063E-16,1.));
#18282=DIRECTION('center_axis',(1.,0.,0.));
#18283=DIRECTION('ref_axis',(0.,-0.587785252292473,0.809016994374947));
#18284=DIRECTION('',(0.,-0.587785252292473,-0.809016994374947));
#18285=DIRECTION('',(0.,0.587785252292473,0.809016994374947));
#18286=DIRECTION('center_axis',(0.,-0.809016994374947,0.587785252292473));
#18287=DIRECTION('ref_axis',(0.,-0.587785252292473,-0.809016994374947));
#18288=DIRECTION('center_axis',(0.,0.809016994374947,-0.587785252292473));
#18289=DIRECTION('ref_axis',(0.,0.587785252292473,0.809016994374947));
#18290=DIRECTION('center_axis',(1.,0.,0.));
#18291=DIRECTION('ref_axis',(0.,1.22464679914735E-16,1.));
#18292=DIRECTION('',(0.,-0.951056516295154,-0.309016994374947));
#18293=DIRECTION('',(0.,0.951056516295154,0.309016994374947));
#18294=DIRECTION('center_axis',(0.,-0.309016994374947,0.951056516295154));
#18295=DIRECTION('ref_axis',(0.,-0.951056516295154,-0.309016994374947));
#18296=DIRECTION('center_axis',(0.,0.309016994374947,-0.951056516295154));
#18297=DIRECTION('ref_axis',(0.,0.951056516295154,0.309016994374947));
#18298=DIRECTION('center_axis',(1.,0.,0.));
#18299=DIRECTION('ref_axis',(0.,0.587785252292473,0.809016994374947));
#18300=DIRECTION('',(0.,-0.951056516295153,0.309016994374948));
#18301=DIRECTION('',(0.,0.951056516295153,-0.309016994374948));
#18302=DIRECTION('center_axis',(0.,0.309016994374948,0.951056516295154));
#18303=DIRECTION('ref_axis',(0.,-0.951056516295153,0.309016994374948));
#18304=DIRECTION('center_axis',(0.,-0.309016994374948,-0.951056516295154));
#18305=DIRECTION('ref_axis',(0.,0.951056516295153,-0.309016994374948));
#18306=DIRECTION('center_axis',(1.,0.,0.));
#18307=DIRECTION('ref_axis',(0.,0.951056516295154,0.309016994374947));
#18308=DIRECTION('',(0.,-0.587785252292473,0.809016994374948));
#18309=DIRECTION('',(0.,0.587785252292473,-0.809016994374947));
#18310=DIRECTION('center_axis',(0.,0.809016994374948,0.587785252292473));
#18311=DIRECTION('ref_axis',(0.,-0.587785252292473,0.809016994374947));
#18312=DIRECTION('center_axis',(0.,-0.809016994374948,-0.587785252292473));
#18313=DIRECTION('ref_axis',(0.,0.587785252292473,-0.809016994374948));
#18314=DIRECTION('center_axis',(1.,0.,0.));
#18315=DIRECTION('ref_axis',(0.,0.951056516295154,-0.309016994374948));
#18316=DIRECTION('',(0.,3.33066907387547E-16,1.));
#18317=DIRECTION('',(0.,-5.55111512312578E-17,-1.));
#18318=DIRECTION('center_axis',(0.,1.,-5.55111512312578E-17));
#18319=DIRECTION('ref_axis',(0.,5.55111512312578E-17,1.));
#18320=DIRECTION('center_axis',(0.,-1.,3.33066907387547E-16));
#18321=DIRECTION('ref_axis',(0.,-3.33066907387547E-16,-1.));
#18322=DIRECTION('center_axis',(1.,0.,0.));
#18323=DIRECTION('ref_axis',(0.,0.587785252292473,-0.809016994374947));
#18324=DIRECTION('',(0.,0.587785252292473,0.809016994374947));
#18325=DIRECTION('',(0.,-0.587785252292473,-0.809016994374947));
#18326=DIRECTION('center_axis',(0.,0.809016994374947,-0.587785252292473));
#18327=DIRECTION('ref_axis',(0.,0.587785252292473,0.809016994374947));
#18328=DIRECTION('center_axis',(0.,-0.809016994374947,0.587785252292473));
#18329=DIRECTION('ref_axis',(0.,-0.587785252292473,-0.809016994374947));
#18330=DIRECTION('center_axis',(0.,0.309016994374947,-0.951056516295154));
#18331=DIRECTION('ref_axis',(0.,0.951056516295154,0.309016994374947));
#18332=DIRECTION('',(1.,0.,0.));
#18333=DIRECTION('',(0.,-0.951056516295154,-0.309016994374947));
#18334=DIRECTION('center_axis',(0.,-0.309016994374947,0.951056516295154));
#18335=DIRECTION('ref_axis',(0.,-0.951056516295154,-0.309016994374947));
#18336=DIRECTION('',(-1.,0.,0.));
#18337=DIRECTION('',(0.,0.951056516295154,0.309016994374947));
#18338=DIRECTION('center_axis',(1.,0.,0.));
#18339=DIRECTION('ref_axis',(0.,0.,-1.));
#18340=DIRECTION('',(0.,0.309016994374948,-0.951056516295153));
#18341=DIRECTION('center_axis',(0.,0.951056516295154,0.309016994374948));
#18342=DIRECTION('ref_axis',(0.,-0.309016994374948,0.951056516295153));
#18343=DIRECTION('',(0.,0.,1.));
#18344=DIRECTION('',(1.,0.,0.));
#18345=DIRECTION('',(0.,0.,1.));
#18346=DIRECTION('',(1.,0.,0.));
#18347=DIRECTION('',(0.,0.,1.));
#18348=DIRECTION('',(1.,0.,0.));
#18349=DIRECTION('',(0.,1.,0.));
#18350=DIRECTION('',(-1.,0.,0.));
#18351=DIRECTION('',(0.,0.,1.));
#18352=DIRECTION('',(1.,0.,0.));
#18353=DIRECTION('',(0.,0.,1.));
#18354=DIRECTION('',(1.,0.,0.));
#18355=DIRECTION('',(0.,0.,1.));
#18356=DIRECTION('',(1.,0.,0.));
#18357=DIRECTION('',(0.,1.,0.));
#18358=DIRECTION('',(-1.,0.,0.));
#18359=DIRECTION('',(0.,-1.,0.));
#18360=DIRECTION('',(0.,0.,1.));
#18361=DIRECTION('',(0.,1.,0.));
#18362=DIRECTION('',(-1.,0.,0.));
#18363=DIRECTION('',(0.,0.,1.));
#18364=DIRECTION('',(0.,1.,0.));
#18365=DIRECTION('',(0.,1.,0.));
#18366=DIRECTION('',(-1.,0.,0.));
#18367=DIRECTION('',(0.,1.,0.));
#18368=DIRECTION('',(-1.,0.,0.));
#18369=DIRECTION('',(0.,1.,0.));
#18370=DIRECTION('',(-1.,0.,0.));
#18371=DIRECTION('',(0.,1.,0.));
#18372=DIRECTION('',(-1.,0.,0.));
#18373=DIRECTION('',(0.,1.,0.));
#18374=DIRECTION('',(-1.,0.,0.));
#18375=DIRECTION('',(0.,1.,0.));
#18376=DIRECTION('',(-1.,0.,0.));
#18377=CARTESIAN_POINT('',(0.,0.,0.));
#18378=CARTESIAN_POINT('',(0.,0.,0.));
#18379=CARTESIAN_POINT('Origin',(177.55,58.9875,12.375));
#18380=CARTESIAN_POINT('',(177.3,58.7375,-24.75));
#18381=CARTESIAN_POINT('',(177.8,59.2375,-24.75));
#18382=CARTESIAN_POINT('',(177.3,58.7375,-24.75));
#18383=CARTESIAN_POINT('',(177.8,59.2375,24.75));
#18384=CARTESIAN_POINT('',(177.8,59.2375,12.375));
#18385=CARTESIAN_POINT('',(177.3,58.7375,24.75));
#18386=CARTESIAN_POINT('',(177.8,59.2375,24.75));
#18387=CARTESIAN_POINT('',(177.3,58.7375,12.375));
#18388=CARTESIAN_POINT('Origin',(177.55,56.5,-24.75));
#18389=CARTESIAN_POINT('',(177.3,56.5,-26.9875));
#18390=CARTESIAN_POINT('',(177.8,56.5,-27.4875));
#18391=CARTESIAN_POINT('',(177.3,56.5,-26.9875));
#18392=CARTESIAN_POINT('Origin',(177.8,56.5,-24.75));
#18393=CARTESIAN_POINT('Origin',(177.3,56.5,-24.75));
#18394=CARTESIAN_POINT('Origin',(177.55,44.125,-27.2375));
#18395=CARTESIAN_POINT('',(177.3,7.,-26.9875));
#18396=CARTESIAN_POINT('',(177.8,7.,-27.4875));
#18397=CARTESIAN_POINT('',(177.3,7.,-26.9875));
#18398=CARTESIAN_POINT('',(177.8,44.125,-27.4875));
#18399=CARTESIAN_POINT('',(177.3,44.125,-26.9875));
#18400=CARTESIAN_POINT('Origin',(177.55,7.,-24.75));
#18401=CARTESIAN_POINT('',(177.3,4.7625,-24.75));
#18402=CARTESIAN_POINT('',(177.8,4.2625,-24.75));
#18403=CARTESIAN_POINT('',(177.3,4.7625,-24.75));
#18404=CARTESIAN_POINT('Origin',(177.8,7.,-24.75));
#18405=CARTESIAN_POINT('Origin',(177.3,7.,-24.75));
#18406=CARTESIAN_POINT('Origin',(177.55,4.5125,-12.375));
#18407=CARTESIAN_POINT('',(177.3,4.7625,24.75));
#18408=CARTESIAN_POINT('',(177.8,4.2625,24.75));
#18409=CARTESIAN_POINT('',(177.3,4.7625,24.75));
#18410=CARTESIAN_POINT('',(177.8,4.2625,-12.375));
#18411=CARTESIAN_POINT('',(177.3,4.7625,-12.375));
#18412=CARTESIAN_POINT('Origin',(177.55,7.,24.75));
#18413=CARTESIAN_POINT('',(177.3,7.,26.9875));
#18414=CARTESIAN_POINT('',(177.8,7.,27.4875));
#18415=CARTESIAN_POINT('',(177.3,7.,26.9875));
#18416=CARTESIAN_POINT('Origin',(177.8,7.,24.75));
#18417=CARTESIAN_POINT('Origin',(177.3,7.,24.75));
#18418=CARTESIAN_POINT('Origin',(177.55,19.375,27.2375));
#18419=CARTESIAN_POINT('',(177.3,56.5,26.9875));
#18420=CARTESIAN_POINT('',(177.8,56.5,27.4875));
#18421=CARTESIAN_POINT('',(177.3,56.5,26.9875));
#18422=CARTESIAN_POINT('',(177.8,19.375,27.4875));
#18423=CARTESIAN_POINT('',(177.3,19.375,26.9875));
#18424=CARTESIAN_POINT('Origin',(177.55,56.5,24.75));
#18425=CARTESIAN_POINT('Origin',(177.8,56.5,24.75));
#18426=CARTESIAN_POINT('Origin',(177.3,56.5,24.75));
#18427=CARTESIAN_POINT('Origin',(0.,7.,-24.75));
#18428=CARTESIAN_POINT('',(0.6,7.,-26.9875));
#18429=CARTESIAN_POINT('',(0.,7.,-26.9875));
#18430=CARTESIAN_POINT('',(0.6,4.7625,-24.75));
#18431=CARTESIAN_POINT('Origin',(0.6,7.,-24.75));
#18432=CARTESIAN_POINT('',(0.,4.7625,-24.75));
#18433=CARTESIAN_POINT('Origin',(0.,56.5,-26.9875));
#18434=CARTESIAN_POINT('',(0.6,56.5,-26.9875));
#18435=CARTESIAN_POINT('',(0.,56.5,-26.9875));
#18436=CARTESIAN_POINT('',(0.6,44.125,-26.9875));
#18437=CARTESIAN_POINT('',(10.,31.75,-26.9875));
#18438=CARTESIAN_POINT('Origin',(15.2,31.75,-26.9875));
#18439=CARTESIAN_POINT('Origin',(0.,56.5,-24.75));
#18440=CARTESIAN_POINT('',(0.6,58.7375,-24.75));
#18441=CARTESIAN_POINT('',(0.,58.7375,-24.75));
#18442=CARTESIAN_POINT('Origin',(0.6,56.5,-24.75));
#18443=CARTESIAN_POINT('Origin',(0.,58.7375,24.75));
#18444=CARTESIAN_POINT('',(0.6,58.7375,24.75));
#18445=CARTESIAN_POINT('',(0.,58.7375,24.75));
#18446=CARTESIAN_POINT('',(0.6,58.7375,12.375));
#18447=CARTESIAN_POINT('Origin',(177.8,31.75,0.));
#18448=CARTESIAN_POINT('',(177.8,7.,31.25));
#18449=CARTESIAN_POINT('',(177.8,56.5,31.25));
#18450=CARTESIAN_POINT('',(177.8,44.125,31.25));
#18451=CARTESIAN_POINT('',(177.8,0.499999999999998,24.75));
#18452=CARTESIAN_POINT('Origin',(177.8,7.,24.75));
#18453=CARTESIAN_POINT('',(177.8,0.5,-24.75));
#18454=CARTESIAN_POINT('',(177.8,0.5,12.375));
#18455=CARTESIAN_POINT('',(177.8,7.,-31.25));
#18456=CARTESIAN_POINT('Origin',(177.8,7.,-24.75));
#18457=CARTESIAN_POINT('',(177.8,56.5,-31.25));
#18458=CARTESIAN_POINT('',(177.8,19.375,-31.25));
#18459=CARTESIAN_POINT('',(177.8,63.,-24.75));
#18460=CARTESIAN_POINT('Origin',(177.8,56.5,-24.75));
#18461=CARTESIAN_POINT('',(177.8,63.,24.75));
#18462=CARTESIAN_POINT('',(177.8,63.,-12.375));
#18463=CARTESIAN_POINT('Origin',(177.8,56.5,24.75));
#18464=CARTESIAN_POINT('Origin',(177.55,44.125,31.5));
#18465=CARTESIAN_POINT('',(177.3,7.,31.75));
#18466=CARTESIAN_POINT('',(177.3,7.,31.75));
#18467=CARTESIAN_POINT('',(177.3,56.5,31.75));
#18468=CARTESIAN_POINT('',(177.8,56.5,31.25));
#18469=CARTESIAN_POINT('',(177.3,44.125,31.75));
#18470=CARTESIAN_POINT('Origin',(177.55,7.,24.75));
#18471=CARTESIAN_POINT('',(177.3,-1.11022302462516E-15,24.75));
#18472=CARTESIAN_POINT('',(177.3,-1.11022302462516E-15,24.75));
#18473=CARTESIAN_POINT('Origin',(177.3,7.,24.75));
#18474=CARTESIAN_POINT('Origin',(177.55,0.25,12.375));
#18475=CARTESIAN_POINT('',(177.3,0.,-24.75));
#18476=CARTESIAN_POINT('',(177.3,0.,-24.75));
#18477=CARTESIAN_POINT('',(177.3,0.,12.375));
#18478=CARTESIAN_POINT('Origin',(177.55,7.,-24.75));
#18479=CARTESIAN_POINT('',(177.3,7.,-31.75));
#18480=CARTESIAN_POINT('',(177.3,7.,-31.75));
#18481=CARTESIAN_POINT('Origin',(177.3,7.,-24.75));
#18482=CARTESIAN_POINT('Origin',(177.55,19.375,-31.5));
#18483=CARTESIAN_POINT('',(177.3,56.5,-31.75));
#18484=CARTESIAN_POINT('',(177.3,56.5,-31.75));
#18485=CARTESIAN_POINT('',(177.3,19.375,-31.75));
#18486=CARTESIAN_POINT('Origin',(177.55,56.5,-24.75));
#18487=CARTESIAN_POINT('',(177.3,63.5,-24.75));
#18488=CARTESIAN_POINT('',(177.3,63.5,-24.75));
#18489=CARTESIAN_POINT('Origin',(177.3,56.5,-24.75));
#18490=CARTESIAN_POINT('Origin',(177.55,63.25,-12.375));
#18491=CARTESIAN_POINT('',(177.3,63.5,24.75));
#18492=CARTESIAN_POINT('',(177.3,63.5,24.75));
#18493=CARTESIAN_POINT('',(177.3,63.5,-12.375));
#18494=CARTESIAN_POINT('Origin',(177.55,56.5,24.75));
#18495=CARTESIAN_POINT('Origin',(177.3,56.5,24.75));
#18496=CARTESIAN_POINT('Origin',(0.,7.,-24.75));
#18497=CARTESIAN_POINT('',(0.6,0.,-24.75));
#18498=CARTESIAN_POINT('',(0.,0.,-24.75));
#18499=CARTESIAN_POINT('',(0.6,7.,-31.75));
#18500=CARTESIAN_POINT('Origin',(0.6,7.,-24.75));
#18501=CARTESIAN_POINT('',(0.,7.,-31.75));
#18502=CARTESIAN_POINT('Origin',(0.,0.,24.75));
#18503=CARTESIAN_POINT('',(0.6,-1.11022302462516E-15,24.75));
#18504=CARTESIAN_POINT('',(0.,-1.11022302462516E-15,24.75));
#18505=CARTESIAN_POINT('',(0.6,0.,12.375));
#18506=CARTESIAN_POINT('Origin',(0.,7.,24.75));
#18507=CARTESIAN_POINT('',(0.6,7.,31.75));
#18508=CARTESIAN_POINT('',(0.,7.,31.75));
#18509=CARTESIAN_POINT('Origin',(0.6,7.,24.75));
#18510=CARTESIAN_POINT('Origin',(0.,56.5,31.75));
#18511=CARTESIAN_POINT('',(0.6,56.5,31.75));
#18512=CARTESIAN_POINT('',(0.,56.5,31.75));
#18513=CARTESIAN_POINT('',(0.6,44.125,31.75));
#18514=CARTESIAN_POINT('Origin',(0.3,0.3,12.375));
#18515=CARTESIAN_POINT('',(0.,0.600000000000001,-24.75));
#18516=CARTESIAN_POINT('',(0.,0.600000000000001,-24.75));
#18517=CARTESIAN_POINT('',(0.,0.600000000000001,24.75));
#18518=CARTESIAN_POINT('',(0.6,-1.11022302462516E-15,24.75));
#18519=CARTESIAN_POINT('',(0.,0.600000000000001,12.375));
#18520=CARTESIAN_POINT('Origin',(0.3,7.,-24.75));
#18521=CARTESIAN_POINT('',(0.,7.,-31.15));
#18522=CARTESIAN_POINT('',(0.,7.,-31.15));
#18523=CARTESIAN_POINT('Origin',(0.,7.,-24.75));
#18524=CARTESIAN_POINT('Origin',(0.3,19.375,-31.45));
#18525=CARTESIAN_POINT('',(0.,56.5,-31.15));
#18526=CARTESIAN_POINT('',(0.6,56.5,-31.75));
#18527=CARTESIAN_POINT('',(0.,56.5,-31.15));
#18528=CARTESIAN_POINT('',(0.6,19.375,-31.75));
#18529=CARTESIAN_POINT('',(0.,19.375,-31.15));
#18530=CARTESIAN_POINT('Origin',(0.3,56.5,-24.75));
#18531=CARTESIAN_POINT('',(0.,62.9,-24.75));
#18532=CARTESIAN_POINT('',(0.6,63.5,-24.75));
#18533=CARTESIAN_POINT('',(0.,62.9,-24.75));
#18534=CARTESIAN_POINT('Origin',(0.6,56.5,-24.75));
#18535=CARTESIAN_POINT('Origin',(0.,56.5,-24.75));
#18536=CARTESIAN_POINT('Origin',(0.3,63.2,-12.375));
#18537=CARTESIAN_POINT('',(0.,62.9,24.75));
#18538=CARTESIAN_POINT('',(0.6,63.5,24.75));
#18539=CARTESIAN_POINT('',(0.,62.9,24.75));
#18540=CARTESIAN_POINT('',(0.6,63.5,-12.375));
#18541=CARTESIAN_POINT('',(0.,62.9,-12.375));
#18542=CARTESIAN_POINT('Origin',(0.3,56.5,24.75));
#18543=CARTESIAN_POINT('',(0.,56.5,31.15));
#18544=CARTESIAN_POINT('',(0.,56.5,31.15));
#18545=CARTESIAN_POINT('Origin',(0.6,56.5,24.75));
#18546=CARTESIAN_POINT('Origin',(0.,56.5,24.75));
#18547=CARTESIAN_POINT('Origin',(0.3,44.125,31.45));
#18548=CARTESIAN_POINT('',(0.,7.,31.15));
#18549=CARTESIAN_POINT('',(0.,7.,31.15));
#18550=CARTESIAN_POINT('',(0.,44.125,31.15));
#18551=CARTESIAN_POINT('Origin',(0.3,7.,24.75));
#18552=CARTESIAN_POINT('Origin',(0.,7.,24.75));
#18553=CARTESIAN_POINT('Origin',(0.,56.5,24.75));
#18554=CARTESIAN_POINT('',(0.,63.5,24.75));
#18555=CARTESIAN_POINT('Origin',(0.,31.75,0.));
#18556=CARTESIAN_POINT('',(0.,56.5,-27.5875));
#18557=CARTESIAN_POINT('',(0.,7.,-27.5875));
#18558=CARTESIAN_POINT('',(0.,44.125,-27.5875));
#18559=CARTESIAN_POINT('',(0.,59.3375,-24.75));
#18560=CARTESIAN_POINT('Origin',(0.,56.5,-24.75));
#18561=CARTESIAN_POINT('',(0.,59.3375,24.75));
#18562=CARTESIAN_POINT('',(0.,59.3375,12.375));
#18563=CARTESIAN_POINT('',(0.,56.5,27.5875));
#18564=CARTESIAN_POINT('Origin',(0.,56.5,24.75));
#18565=CARTESIAN_POINT('',(0.,7.,27.5875));
#18566=CARTESIAN_POINT('',(0.,19.375,27.5875));
#18567=CARTESIAN_POINT('',(0.,4.1625,24.75));
#18568=CARTESIAN_POINT('Origin',(0.,7.,24.75));
#18569=CARTESIAN_POINT('',(0.,4.1625,-24.75));
#18570=CARTESIAN_POINT('',(0.,4.1625,-12.375));
#18571=CARTESIAN_POINT('Origin',(0.,7.,-24.75));
#18572=CARTESIAN_POINT('Origin',(0.3,44.125,-27.2875));
#18573=CARTESIAN_POINT('',(0.,7.,-27.5875));
#18574=CARTESIAN_POINT('',(0.6,56.5,-26.9875));
#18575=CARTESIAN_POINT('Origin',(0.3,7.,-24.75));
#18576=CARTESIAN_POINT('',(0.,4.1625,-24.75));
#18577=CARTESIAN_POINT('Origin',(0.3,4.4625,-12.375));
#18578=CARTESIAN_POINT('',(0.6,4.7625,24.75));
#18579=CARTESIAN_POINT('',(0.,4.1625,24.75));
#18580=CARTESIAN_POINT('',(0.6,4.7625,-12.375));
#18581=CARTESIAN_POINT('Origin',(0.3,7.,24.75));
#18582=CARTESIAN_POINT('',(0.6,7.,26.9875));
#18583=CARTESIAN_POINT('',(0.,7.,27.5875));
#18584=CARTESIAN_POINT('Origin',(0.6,7.,24.75));
#18585=CARTESIAN_POINT('Origin',(0.3,19.375,27.2875));
#18586=CARTESIAN_POINT('',(0.6,56.5,26.9875));
#18587=CARTESIAN_POINT('',(0.,56.5,27.5875));
#18588=CARTESIAN_POINT('',(0.6,19.375,26.9875));
#18589=CARTESIAN_POINT('Origin',(0.3,56.5,24.75));
#18590=CARTESIAN_POINT('',(0.,59.3375,24.75));
#18591=CARTESIAN_POINT('Origin',(0.6,56.5,24.75));
#18592=CARTESIAN_POINT('Origin',(0.3,59.0375,12.375));
#18593=CARTESIAN_POINT('',(0.,59.3375,-24.75));
#18594=CARTESIAN_POINT('Origin',(0.3,56.5,-24.75));
#18595=CARTESIAN_POINT('Origin',(0.,56.5,24.75));
#18596=CARTESIAN_POINT('',(0.,56.5,26.9875));
#18597=CARTESIAN_POINT('Origin',(15.2,31.75,-31.75));
#18598=CARTESIAN_POINT('',(10.,31.75,-31.75));
#18599=CARTESIAN_POINT('Origin',(15.2,31.75,-31.75));
#18600=CARTESIAN_POINT('',(10.,31.75,-31.75));
#18601=CARTESIAN_POINT('Origin',(0.,7.,26.9875));
#18602=CARTESIAN_POINT('',(0.,7.,26.9875));
#18603=CARTESIAN_POINT('Origin',(0.,7.,24.75));
#18604=CARTESIAN_POINT('',(0.,4.7625,24.75));
#18605=CARTESIAN_POINT('Origin',(0.,4.7625,-24.75));
#18606=CARTESIAN_POINT('Origin',(0.,63.5,-24.75));
#18607=CARTESIAN_POINT('',(0.,63.5,-24.75));
#18608=CARTESIAN_POINT('Origin',(0.,56.5,-24.75));
#18609=CARTESIAN_POINT('',(0.,56.5,-31.75));
#18610=CARTESIAN_POINT('Origin',(0.,7.,-31.75));
#18611=CARTESIAN_POINT('',(0.,0.,0.));
#18612=CARTESIAN_POINT('Ctrl Pts',(178.412949735578,0.0221746991903159,
-101.882758090243));
#18613=CARTESIAN_POINT('Ctrl Pts',(178.423188588538,0.0197124751515442,
-101.853918449636));
#18614=CARTESIAN_POINT('Ctrl Pts',(178.514954119049,-0.000380689216689832,
-101.59747251699));
#18615=CARTESIAN_POINT('Ctrl Pts',(178.592152319935,2.07285186112207E-16,
-101.38857532093));
#18616=CARTESIAN_POINT('Ctrl Pts',(178.6,5.55111512312591E-16,-101.366904810515));
#18617=CARTESIAN_POINT('Ctrl Pts',(178.537808007848,0.014917453309238,-101.928351016583));
#18618=CARTESIAN_POINT('Ctrl Pts',(178.545154918172,0.0138762567563856,
-101.907795776369));
#18619=CARTESIAN_POINT('Ctrl Pts',(178.609866781544,-0.0024252187702473,
-101.725953735215));
#18620=CARTESIAN_POINT('Ctrl Pts',(178.665385999329,1.38099875338694E-16,
-101.576687138619));
#18621=CARTESIAN_POINT('Ctrl Pts',(178.670972086323,3.70074341541732E-16,
-101.561269873677));
#18622=CARTESIAN_POINT('Ctrl Pts',(178.662666280119,0.00766020742816023,
-101.973943942923));
#18623=CARTESIAN_POINT('Ctrl Pts',(178.667057936009,0.00742672667316728,
-101.961748861519));
#18624=CARTESIAN_POINT('Ctrl Pts',(178.706720397631,0.00233113595076795,
-101.85253791136));
#18625=CARTESIAN_POINT('Ctrl Pts',(178.738619678723,6.91866932068973E-17,
-101.764798956307));
#18626=CARTESIAN_POINT('Ctrl Pts',(178.741944172646,1.85037170770872E-16,
-101.755634936838));
#18627=CARTESIAN_POINT('Ctrl Pts',(178.787524552389,0.000402961547082414,
-102.019536869264));
#18628=CARTESIAN_POINT('Ctrl Pts',(178.788941666476,0.000357983627884323,
-102.015656202882));
#18629=CARTESIAN_POINT('Ctrl Pts',(178.801571117716,-7.9890588520116E-6,
-101.981070701652));
#18630=CARTESIAN_POINT('Ctrl Pts',(178.811853358117,1.27573599516211E-29,
-101.952910773995));
#18631=CARTESIAN_POINT('Ctrl Pts',(178.812916258969,1.27573599516211E-29,
-101.95));
#18632=CARTESIAN_POINT('',(178.6,5.55111512312578E-16,-101.366904810515));
#18633=CARTESIAN_POINT('',(178.412949735578,0.0221746991903159,-101.882758090243));
#18634=CARTESIAN_POINT('Ctrl Pts',(178.6,4.44089209850063E-16,-101.366904810515));
#18635=CARTESIAN_POINT('Ctrl Pts',(178.59945852697,4.20005404597354E-16,
-101.368400029082));
#18636=CARTESIAN_POINT('Ctrl Pts',(178.598915538305,5.09286916248376E-7,
-101.369899384534));
#18637=CARTESIAN_POINT('Ctrl Pts',(178.598314541834,1.77548273883055E-6,
-101.37155677101));
#18638=CARTESIAN_POINT('Ctrl Pts',(178.597685600891,3.1005527405874E-6,
-101.373291220818));
#18639=CARTESIAN_POINT('Ctrl Pts',(178.596993140289,5.24993586700169E-6,
-101.375198716009));
#18640=CARTESIAN_POINT('Ctrl Pts',(178.596192315107,9.06159147229246E-6,
-101.377401328991));
#18641=CARTESIAN_POINT('Ctrl Pts',(178.595361925554,1.30139634384334E-5,
-101.379685256686));
#18642=CARTESIAN_POINT('Ctrl Pts',(178.594415090726,1.8748033103421E-5,
-101.382286305868));
#18643=CARTESIAN_POINT('Ctrl Pts',(178.593322100849,2.78719461983545E-5,
-101.385285246245));
#18644=CARTESIAN_POINT('Ctrl Pts',(178.592179791908,3.7407558304085E-5,
-101.388419508032));
#18645=CARTESIAN_POINT('Ctrl Pts',(178.590877924042,5.06497810078656E-5,
-101.391988146604));
#18646=CARTESIAN_POINT('Ctrl Pts',(178.589403202399,7.01856533839029E-5,
-101.396027187129));
#18647=CARTESIAN_POINT('Ctrl Pts',(178.587842980484,9.0854161485207E-5,
-101.400300400026));
#18648=CARTESIAN_POINT('Ctrl Pts',(178.586089389774,0.000118592479514606,
-101.405099836938));
#18649=CARTESIAN_POINT('Ctrl Pts',(178.584147820027,0.000157072676082226,
-101.410410677723));
#18650=CARTESIAN_POINT('Ctrl Pts',(178.5820491216,0.000198667024222329,
-101.41615131785));
#18651=CARTESIAN_POINT('Ctrl Pts',(178.579730945858,0.000252874493260704,
-101.42248904508));
#18652=CARTESIAN_POINT('Ctrl Pts',(178.577222120356,0.000324335621672112,
-101.429345386505));
#18653=CARTESIAN_POINT('Ctrl Pts',(178.574377192256,0.000405370262009153,
-101.437120258995));
#18654=CARTESIAN_POINT('Ctrl Pts',(178.571287400785,0.000508732071868225,
-101.445561210993));
#18655=CARTESIAN_POINT('Ctrl Pts',(178.568018800818,0.000639503791382112,
-101.454488825522));
#18656=CARTESIAN_POINT('Ctrl Pts',(178.562944383933,0.000842523502652618,
-101.468348716107));
#18657=CARTESIAN_POINT('Ctrl Pts',(178.557440800738,0.00111288774644858,
-101.483376639919));
#18658=CARTESIAN_POINT('Ctrl Pts',(178.551802736549,0.00145317996012051,
-101.498773356));
#18659=CARTESIAN_POINT('Ctrl Pts',(178.548206591168,0.0016702296833909,
-101.508593895026));
#18660=CARTESIAN_POINT('Ctrl Pts',(178.544556784656,0.00191520563125934,
-101.518561639214));
#18661=CARTESIAN_POINT('Ctrl Pts',(178.540921312626,0.00218441435491767,
-101.528492379834));
#18662=CARTESIAN_POINT('Ctrl Pts',(178.537513057598,0.00243679753334736,
-101.537802449165));
#18663=CARTESIAN_POINT('Ctrl Pts',(178.534117901125,0.00271033425977986,
-101.54707862243));
#18664=CARTESIAN_POINT('Ctrl Pts',(178.530774591244,0.00300072598369727,
-101.556216272597));
#18665=CARTESIAN_POINT('Ctrl Pts',(178.527853564307,0.00325443924329612,
-101.564199774942));
#18666=CARTESIAN_POINT('Ctrl Pts',(178.524972112737,0.00352092663549996,
-101.572077526154));
#18667=CARTESIAN_POINT('Ctrl Pts',(178.522139893218,0.00379788761149813,
-101.579824088899));
#18668=CARTESIAN_POINT('Ctrl Pts',(178.519478343991,0.00405815884639462,
-101.587103841739));
#18669=CARTESIAN_POINT('Ctrl Pts',(178.516860351853,0.00432761426520865,
-101.594267506857));
#18670=CARTESIAN_POINT('Ctrl Pts',(178.514277900784,0.00460593307088419,
-101.601338094426));
#18671=CARTESIAN_POINT('Ctrl Pts',(178.511799080951,0.00487308321503558,
-101.60812494623));
#18672=CARTESIAN_POINT('Ctrl Pts',(178.509353088197,0.0051483431981555,
-101.614825801238));
#18673=CARTESIAN_POINT('Ctrl Pts',(178.506916399187,0.00543380183925013,
-101.621506458109));
#18674=CARTESIAN_POINT('Ctrl Pts',(178.504429078999,0.00572519193357054,
-101.628325930199));
#18675=CARTESIAN_POINT('Ctrl Pts',(178.50194866006,0.00602751424299315,
-101.635132076566));
#18676=CARTESIAN_POINT('Ctrl Pts',(178.499444122459,0.00634483842667621,
-101.642011678311));
#18677=CARTESIAN_POINT('Ctrl Pts',(178.496859738753,0.00667227908863532,
-101.649110605734));
#18678=CARTESIAN_POINT('Ctrl Pts',(178.494249748556,0.0070157416033647,
-101.656287555538));
#18679=CARTESIAN_POINT('Ctrl Pts',(178.491600508035,0.00737805345699072,
-101.663581424513));
#18680=CARTESIAN_POINT('Ctrl Pts',(178.488804043098,0.00776049981719095,
-101.671280630633));
#18681=CARTESIAN_POINT('Ctrl Pts',(178.485963965907,0.00816399903704424,
-101.679109797114));
#18682=CARTESIAN_POINT('Ctrl Pts',(178.483084972836,0.00858931241530336,
-101.68705709765));
#18683=CARTESIAN_POINT('Ctrl Pts',(178.479986355456,0.00904707087224558,
-101.695610658898));
#18684=CARTESIAN_POINT('Ctrl Pts',(178.476842835217,0.00953016315957769,
-101.704300612999));
#18685=CARTESIAN_POINT('Ctrl Pts',(178.47368140586,0.0100356889235731,-101.713053049961));
#18686=CARTESIAN_POINT('Ctrl Pts',(178.470120265003,0.0106051302265015,
-101.722912090711));
#18687=CARTESIAN_POINT('Ctrl Pts',(178.466536704481,0.0112031337716295,
-101.732849644034));
#18688=CARTESIAN_POINT('Ctrl Pts',(178.462991613128,0.011819372271303,-101.742696590626));
#18689=CARTESIAN_POINT('Ctrl Pts',(178.456316716467,0.0129796606517407,
-101.761236973481));
#18690=CARTESIAN_POINT('Ctrl Pts',(178.449781177082,0.0142069873144255,
-101.779449700228));
#18691=CARTESIAN_POINT('Ctrl Pts',(178.443867730057,0.0153837152578814,
-101.795972224341));
#18692=CARTESIAN_POINT('Ctrl Pts',(178.440842416488,0.0159857280940882,
-101.804425131113));
#18693=CARTESIAN_POINT('Ctrl Pts',(178.437980334388,0.0165735927382017,
-101.812433997959));
#18694=CARTESIAN_POINT('Ctrl Pts',(178.435334953384,0.0171300092461038,
-101.819845063868));
#18695=CARTESIAN_POINT('Ctrl Pts',(178.432951108472,0.0176314155309591,
-101.826523433348));
#18696=CARTESIAN_POINT('Ctrl Pts',(178.430743438668,0.0181071457819583,
-101.832715725971));
#18697=CARTESIAN_POINT('Ctrl Pts',(178.428737030369,0.0185468694585307,
-101.838348235259));
#18698=CARTESIAN_POINT('Ctrl Pts',(178.426860560632,0.0189581158494036,
-101.843615973249));
#18699=CARTESIAN_POINT('Ctrl Pts',(178.425160261885,0.0193377870550568,
-101.848393671963));
#18700=CARTESIAN_POINT('Ctrl Pts',(178.423641411031,0.0196810600166027,
-101.852663957193));
#18701=CARTESIAN_POINT('Ctrl Pts',(178.422228645277,0.020000356860667,-101.856635981645));
#18702=CARTESIAN_POINT('Ctrl Pts',(178.420972900558,0.0202881342051908,
-101.860168883262));
#18703=CARTESIAN_POINT('Ctrl Pts',(178.419863717692,0.0205444722138255,
-101.863290454144));
#18704=CARTESIAN_POINT('Ctrl Pts',(178.418788174717,0.0207930358664343,
-101.866317352357));
#18705=CARTESIAN_POINT('Ctrl Pts',(178.417850536333,0.0210120087344738,
-101.868957207664));
#18706=CARTESIAN_POINT('Ctrl Pts',(178.417025849348,0.0212057651772088,
-101.871279308984));
#18707=CARTESIAN_POINT('Ctrl Pts',(178.416222831459,0.0213944305649158,
-101.87354039584));
#18708=CARTESIAN_POINT('Ctrl Pts',(178.415526991626,0.0215591700668775,
-101.875499968855));
#18709=CARTESIAN_POINT('Ctrl Pts',(178.414899116768,0.0217084973953576,
-101.877268125753));
#18710=CARTESIAN_POINT('Ctrl Pts',(178.414290865431,0.0218531576661837,
-101.878981020896));
#18711=CARTESIAN_POINT('Ctrl Pts',(178.41374644488,0.0219833464708782,-101.880514144137));
#18712=CARTESIAN_POINT('Ctrl Pts',(178.413213893231,0.0221112223987379,
-101.88201406864));
#18713=CARTESIAN_POINT('Ctrl Pts',(178.413125647366,0.0221324119336719,
-101.882262611921));
#18714=CARTESIAN_POINT('Ctrl Pts',(178.413037689107,0.0221535482572281,
-101.88251035271));
#18715=CARTESIAN_POINT('Ctrl Pts',(178.412949735578,0.0221746991903141,
-101.882758090243));
#18716=CARTESIAN_POINT('',(178.787524552389,0.000402961547082414,-102.019536869264));
#18717=CARTESIAN_POINT('Ctrl Pts',(178.787524552389,0.000402961547082414,
-102.019536869264));
#18718=CARTESIAN_POINT('Ctrl Pts',(178.662666280119,0.00766020742816023,
-101.973943942923));
#18719=CARTESIAN_POINT('Ctrl Pts',(178.537808007848,0.014917453309238,-101.928351016583));
#18720=CARTESIAN_POINT('Ctrl Pts',(178.412949735578,0.0221746991903159,
-101.882758090243));
#18721=CARTESIAN_POINT('',(178.812916258969,0.,-101.95));
#18722=CARTESIAN_POINT('Ctrl Pts',(178.787524552389,0.000402961547083081,
-102.019536869264));
#18723=CARTESIAN_POINT('Ctrl Pts',(178.78764841214,0.000399030350633984,
-102.019197688124));
#18724=CARTESIAN_POINT('Ctrl Pts',(178.787773880524,0.000395071002771159,
-102.01885410166));
#18725=CARTESIAN_POINT('Ctrl Pts',(178.78793361532,0.000390082847545159,
-102.018416679296));
#18726=CARTESIAN_POINT('Ctrl Pts',(178.788100783821,0.000384862554586033,
-102.017958900261));
#18727=CARTESIAN_POINT('Ctrl Pts',(178.788305342406,0.000378518970205901,
-102.01739873139));
#18728=CARTESIAN_POINT('Ctrl Pts',(178.788564734392,0.000370623383797231,
-102.016688404118));
#18729=CARTESIAN_POINT('Ctrl Pts',(178.788858149117,0.000361692185276813,
-102.015884907893));
#18730=CARTESIAN_POINT('Ctrl Pts',(178.789221715781,0.000350777275430554,
-102.014889304208));
#18731=CARTESIAN_POINT('Ctrl Pts',(178.789656465201,0.00033813726450127,
-102.013698766371));
#18732=CARTESIAN_POINT('Ctrl Pts',(178.790132138563,0.000324307420864918,
-102.012396160525));
#18733=CARTESIAN_POINT('Ctrl Pts',(178.790692580633,0.000308441360554114,
-102.010861415125));
#18734=CARTESIAN_POINT('Ctrl Pts',(178.791315549691,0.000291620850831009,
-102.009155432272));
#18735=CARTESIAN_POINT('Ctrl Pts',(178.792247224669,0.000266465110246515,
-102.006604067135));
#18736=CARTESIAN_POINT('Ctrl Pts',(178.793317070051,0.000239334836013709,
-102.003674304649));
#18737=CARTESIAN_POINT('Ctrl Pts',(178.794410700059,0.00021403709302259,
-102.000679377506));
#18738=CARTESIAN_POINT('Ctrl Pts',(178.795148224044,0.000196976759901188,
-101.998659653661));
#18739=CARTESIAN_POINT('Ctrl Pts',(178.795895454195,0.000180736351586767,
-101.9966133361));
#18740=CARTESIAN_POINT('Ctrl Pts',(178.796625704937,0.000165866021982986,
-101.994613504147));
#18741=CARTESIAN_POINT('Ctrl Pts',(178.797262035433,0.000152908220404063,
-101.992870877969));
#18742=CARTESIAN_POINT('Ctrl Pts',(178.797885231353,0.000140979679693556,
-101.991164211473));
#18743=CARTESIAN_POINT('Ctrl Pts',(178.798491417233,0.000130049363544771,
-101.989504119402));
#18744=CARTESIAN_POINT('Ctrl Pts',(178.799058386644,0.000119826171107409,
-101.987951424998));
#18745=CARTESIAN_POINT('Ctrl Pts',(178.799610286814,0.000110468349953339,
-101.986439991158));
#18746=CARTESIAN_POINT('Ctrl Pts',(178.800159818369,0.000101705604670599,
-101.984935038457));
#18747=CARTESIAN_POINT('Ctrl Pts',(178.800710252065,9.29284739725731E-5,
-101.983427615142));
#18748=CARTESIAN_POINT('Ctrl Pts',(178.801261406613,8.46980848399352E-5,
-101.981918212337));
#18749=CARTESIAN_POINT('Ctrl Pts',(178.801827369149,7.68530597206052E-5,
-101.980368253329));
#18750=CARTESIAN_POINT('Ctrl Pts',(178.802440098241,6.8359785321794E-5,
-101.978690218273));
#18751=CARTESIAN_POINT('Ctrl Pts',(178.803070001693,6.03342640516636E-5,
-101.976965145865));
#18752=CARTESIAN_POINT('Ctrl Pts',(178.803714099497,5.29252697356597E-5,
-101.975201199093));
#18753=CARTESIAN_POINT('Ctrl Pts',(178.804466950208,4.42653013113147E-5,
-101.973139418143));
#18754=CARTESIAN_POINT('Ctrl Pts',(178.805238896389,3.64757779670852E-5,
-101.971025339937));
#18755=CARTESIAN_POINT('Ctrl Pts',(178.806001069089,2.98874832731499E-5,
-101.968938028039));
#18756=CARTESIAN_POINT('Ctrl Pts',(178.806915993951,2.19787840815128E-5,
-101.96643238391));
#18757=CARTESIAN_POINT('Ctrl Pts',(178.807815215869,1.58466567429737E-5,
-101.963969744905));
#18758=CARTESIAN_POINT('Ctrl Pts',(178.808631227751,1.14758459881514E-5,
-101.961734991272));
#18759=CARTESIAN_POINT('Ctrl Pts',(178.809260196792,8.1068942553096E-6,
-101.960012478552));
#18760=CARTESIAN_POINT('Ctrl Pts',(178.809838942981,5.75949614264358E-6,
-101.958427509956));
#18761=CARTESIAN_POINT('Ctrl Pts',(178.810343455118,4.13699453183369E-6,
-101.957045843971));
#18762=CARTESIAN_POINT('Ctrl Pts',(178.810801738817,2.66316271661563E-6,
-101.955790780017));
#18763=CARTESIAN_POINT('Ctrl Pts',(178.811198450184,1.77620580733071E-6,
-101.95470434237));
#18764=CARTESIAN_POINT('Ctrl Pts',(178.811528375133,1.20384667301465E-6,
-101.953800810259));
#18765=CARTESIAN_POINT('Ctrl Pts',(178.811837957088,6.66778893284302E-7,
-101.95295298945));
#18766=CARTESIAN_POINT('Ctrl Pts',(178.812088533466,4.02530379490208E-7,
-101.952266765043));
#18767=CARTESIAN_POINT('Ctrl Pts',(178.812291139739,2.44220887957169E-7,
-101.951711914309));
#18768=CARTESIAN_POINT('Ctrl Pts',(178.812480730277,9.60814393472537E-8,
-101.951192708032));
#18769=CARTESIAN_POINT('Ctrl Pts',(178.812628230417,4.12488927176395E-8,
-101.950788772916));
#18770=CARTESIAN_POINT('Ctrl Pts',(178.812758452829,1.55631960652158E-8,
-101.950432155475));
#18771=CARTESIAN_POINT('Ctrl Pts',(178.812812952405,4.81343668080793E-9,
-101.950282906975));
#18772=CARTESIAN_POINT('Ctrl Pts',(178.812864631041,0.,-101.950141384054));
#18773=CARTESIAN_POINT('Ctrl Pts',(178.812916258969,0.,-101.95));
#18774=CARTESIAN_POINT('',(178.706458129484,2.77555756156289E-16,-101.658452405258));
#18775=CARTESIAN_POINT('Ctrl Pts',(178.787524039848,5.93046172723724,-107.949597022186));
#18776=CARTESIAN_POINT('Ctrl Pts',(178.788055468328,5.9319170065127,-107.949613889587));
#18777=CARTESIAN_POINT('Ctrl Pts',(178.789730276056,5.93650327150383,-107.94967251859));
#18778=CARTESIAN_POINT('Ctrl Pts',(178.796663949731,5.95549109773913,-107.949843338737));
#18779=CARTESIAN_POINT('Ctrl Pts',(178.802274889545,5.9708572965487,-107.949940304033));
#18780=CARTESIAN_POINT('Ctrl Pts',(178.808321541956,5.98741690531324,-107.949992199559));
#18781=CARTESIAN_POINT('Ctrl Pts',(178.811886383268,5.99717964379856,-107.950000306293));
#18782=CARTESIAN_POINT('Ctrl Pts',(178.812561951533,5.99902972241609,-107.95));
#18783=CARTESIAN_POINT('Ctrl Pts',(178.812916258969,6.,-107.95));
#18784=CARTESIAN_POINT('Ctrl Pts',(178.662665771413,5.97605465101009,-107.942339741564));
#18785=CARTESIAN_POINT('Ctrl Pts',(178.664312652826,5.98062783599467,-107.942427298381));
#18786=CARTESIAN_POINT('Ctrl Pts',(178.670769881366,5.99845250694587,-107.943108688047));
#18787=CARTESIAN_POINT('Ctrl Pts',(178.689813167772,6.05087787990199,-107.94503083354));
#18788=CARTESIAN_POINT('Ctrl Pts',(178.70976624133,6.1058117496159,-107.947239781462));
#18789=CARTESIAN_POINT('Ctrl Pts',(178.727201696273,6.15378129306144,-107.948897276685));
#18790=CARTESIAN_POINT('Ctrl Pts',(178.737862493431,6.18311815560049,-107.949788255786));
#18791=CARTESIAN_POINT('Ctrl Pts',(178.740836000836,6.19131037031829,-107.95));
#18792=CARTESIAN_POINT('Ctrl Pts',(178.741944172646,6.1943650631615,-107.95));
#18793=CARTESIAN_POINT('Ctrl Pts',(178.537807502978,6.02164757478294,-107.935082460943));
#18794=CARTESIAN_POINT('Ctrl Pts',(178.540562604801,6.02935581973102,-107.935472908878));
#18795=CARTESIAN_POINT('Ctrl Pts',(178.548140009852,6.05016876508724,-107.93751448423));
#18796=CARTESIAN_POINT('Ctrl Pts',(178.587637169058,6.15753734426006,-107.942617344146));
#18797=CARTESIAN_POINT('Ctrl Pts',(178.614548799958,6.23191679011827,-107.946864743799));
#18798=CARTESIAN_POINT('Ctrl Pts',(178.64762791374,6.32331090469419,-107.948970766507));
#18799=CARTESIAN_POINT('Ctrl Pts',(178.666539875963,6.37617477796488,-107.949592686699));
#18800=CARTESIAN_POINT('Ctrl Pts',(178.669110050139,6.3835910182205,-107.95));
#18801=CARTESIAN_POINT('Ctrl Pts',(178.670972086323,6.38873012632301,-107.95));
#18802=CARTESIAN_POINT('Ctrl Pts',(178.412949234542,6.06724049855578,-107.927825180321));
#18803=CARTESIAN_POINT('Ctrl Pts',(178.416788814167,6.07805539364222,-107.9287485193));
#18804=CARTESIAN_POINT('Ctrl Pts',(178.428797505081,6.11209602694949,-107.931943728692));
#18805=CARTESIAN_POINT('Ctrl Pts',(178.47931211943,6.25289954945229,-107.941313577143));
#18806=CARTESIAN_POINT('Ctrl Pts',(178.520871373432,6.36685401704756,-107.946698106754));
#18807=CARTESIAN_POINT('Ctrl Pts',(178.565883366218,6.48966771290196,-107.94957040054));
#18808=CARTESIAN_POINT('Ctrl Pts',(178.592383761069,6.56211168242985,-107.950016726301));
#18809=CARTESIAN_POINT('Ctrl Pts',(178.597384099442,6.57587166612271,-107.95));
#18810=CARTESIAN_POINT('Ctrl Pts',(178.6,6.58309518948451,-107.95));
#18811=CARTESIAN_POINT('',(178.812916258969,6.,-107.95));
#18812=CARTESIAN_POINT('',(178.787524039848,5.93046172723724,-107.949597022186));
#18813=CARTESIAN_POINT('Ctrl Pts',(178.812916258969,6.,-107.95));
#18814=CARTESIAN_POINT('Ctrl Pts',(178.8127923898,5.99966078194887,-107.95));
#18815=CARTESIAN_POINT('Ctrl Pts',(178.812666912034,5.99931715853558,-107.949999977092));
#18816=CARTESIAN_POINT('Ctrl Pts',(178.812507168478,5.99887969296171,-107.949999895409));
#18817=CARTESIAN_POINT('Ctrl Pts',(178.812339990794,5.99842186866603,-107.949999809925));
#18818=CARTESIAN_POINT('Ctrl Pts',(178.812135423695,5.99786164766841,-107.949999661008));
#18819=CARTESIAN_POINT('Ctrl Pts',(178.811876024087,5.99715125904428,-107.949999323723));
#18820=CARTESIAN_POINT('Ctrl Pts',(178.811582600943,5.99634769397784,-107.949998942198));
#18821=CARTESIAN_POINT('Ctrl Pts',(178.811219027098,5.99535200993297,-107.949998317815));
#18822=CARTESIAN_POINT('Ctrl Pts',(178.810784271547,5.99416138284707,-107.949997159212));
#18823=CARTESIAN_POINT('Ctrl Pts',(178.810308592617,5.99285868247457,-107.94999589155));
#18824=CARTESIAN_POINT('Ctrl Pts',(178.809748146635,5.99132383326824,-107.94999396957));
#18825=CARTESIAN_POINT('Ctrl Pts',(178.809125174401,5.98961774499851,-107.949991017392));
#18826=CARTESIAN_POINT('Ctrl Pts',(178.808193484888,5.98706619540862,-107.949986602245));
#18827=CARTESIAN_POINT('Ctrl Pts',(178.807123623593,5.98413623812711,-107.949979775947));
#18828=CARTESIAN_POINT('Ctrl Pts',(178.806029976263,5.98114113876119,-107.949970361873));
#18829=CARTESIAN_POINT('Ctrl Pts',(178.805292443291,5.97912130615377,-107.949964013218));
#18830=CARTESIAN_POINT('Ctrl Pts',(178.8045452036,5.9770748900843,-107.949956536432));
#18831=CARTESIAN_POINT('Ctrl Pts',(178.803814942577,5.97507497391497,-107.949948228366));
#18832=CARTESIAN_POINT('Ctrl Pts',(178.803178603945,5.97333227660838,-107.949940988841));
#18833=CARTESIAN_POINT('Ctrl Pts',(178.802555399287,5.97162554958125,-107.949933136853));
#18834=CARTESIAN_POINT('Ctrl Pts',(178.801949204102,5.96996540809482,-107.94992482647));
#18835=CARTESIAN_POINT('Ctrl Pts',(178.801382229386,5.96841267678133,-107.949917053764));
#18836=CARTESIAN_POINT('Ctrl Pts',(178.800830323213,5.96690121509211,-107.949908893929));
#18837=CARTESIAN_POINT('Ctrl Pts',(178.800280785516,5.96539624482733,-107.949900214181));
#18838=CARTESIAN_POINT('Ctrl Pts',(178.799730342856,5.96388879622168,-107.949891520139));
#18839=CARTESIAN_POINT('Ctrl Pts',(178.799179179282,5.96237937864897,-107.949882256457));
#18840=CARTESIAN_POINT('Ctrl Pts',(178.798613206928,5.96082941367589,-107.949872137401));
#18841=CARTESIAN_POINT('Ctrl Pts',(178.798000470593,5.95915138143477,-107.94986118225));
#18842=CARTESIAN_POINT('Ctrl Pts',(178.797370559173,5.95742632285293,-107.949849214239));
#18843=CARTESIAN_POINT('Ctrl Pts',(178.796726452316,5.95566239958307,-107.949836179196));
#18844=CARTESIAN_POINT('Ctrl Pts',(178.795973597401,5.9536006635722,-107.949820943375));
#18845=CARTESIAN_POINT('Ctrl Pts',(178.795201645861,5.95148664466333,-107.949804231078));
#18846=CARTESIAN_POINT('Ctrl Pts',(178.794439465761,5.94939939913607,-107.949786627805));
#18847=CARTESIAN_POINT('Ctrl Pts',(178.793524504241,5.94689375861677,-107.949765495901));
#18848=CARTESIAN_POINT('Ctrl Pts',(178.79262524356,5.944431135813,-107.949743085817));
#18849=CARTESIAN_POINT('Ctrl Pts',(178.791809196363,5.94219640766138,-107.949721555598));
#18850=CARTESIAN_POINT('Ctrl Pts',(178.791180207509,5.94047393486153,-107.949704960642));
#18851=CARTESIAN_POINT('Ctrl Pts',(178.790601442454,5.9388890082226,-107.949688938252));
#18852=CARTESIAN_POINT('Ctrl Pts',(178.790096914054,5.93750738102304,-107.949674547221));
#18853=CARTESIAN_POINT('Ctrl Pts',(178.789638616417,5.93625235458416,-107.949661474864));
#18854=CARTESIAN_POINT('Ctrl Pts',(178.789241893049,5.93516595105505,-107.949649769988));
#18855=CARTESIAN_POINT('Ctrl Pts',(178.788911959032,5.93426244786692,-107.949639870379));
#18856=CARTESIAN_POINT('Ctrl Pts',(178.788602368806,5.93341465484948,-107.949630581182));
#18857=CARTESIAN_POINT('Ctrl Pts',(178.788351786654,5.93272845333488,-107.949622892056));
#18858=CARTESIAN_POINT('Ctrl Pts',(178.788149177667,5.93217362299574,-107.949616619633));
#18859=CARTESIAN_POINT('Ctrl Pts',(178.787959584857,5.9316544365331,-107.949610750169));
#18860=CARTESIAN_POINT('Ctrl Pts',(178.787812085006,5.93125051870808,-107.949606123405));
#18861=CARTESIAN_POINT('Ctrl Pts',(178.787681865722,5.93089392231775,-107.94960201597));
#18862=CARTESIAN_POINT('Ctrl Pts',(178.787627358605,5.93074465839335,-107.949600296682));
#18863=CARTESIAN_POINT('Ctrl Pts',(178.787575673856,5.9306031233133,-107.949598661036));
#18864=CARTESIAN_POINT('Ctrl Pts',(178.787524039848,5.93046172723724,-107.949597022186));
#18865=CARTESIAN_POINT('',(178.412949234542,6.06724049855578,-107.927825180321));
#18866=CARTESIAN_POINT('Ctrl Pts',(178.412949234542,6.06724049855578,-107.927825180321));
#18867=CARTESIAN_POINT('Ctrl Pts',(178.537807502978,6.02164757478294,-107.935082460943));
#18868=CARTESIAN_POINT('Ctrl Pts',(178.662665771413,5.97605465101009,-107.942339741564));
#18869=CARTESIAN_POINT('Ctrl Pts',(178.787524039848,5.93046172723724,-107.949597022186));
#18870=CARTESIAN_POINT('',(178.6,6.58309518948451,-107.95));
#18871=CARTESIAN_POINT('Ctrl Pts',(178.412949234542,6.06724049855578,-107.927825180321));
#18872=CARTESIAN_POINT('Ctrl Pts',(178.413479203313,6.06873325484981,-107.927952626779));
#18873=CARTESIAN_POINT('Ctrl Pts',(178.414010755826,6.07023015200046,-107.928079922666));
#18874=CARTESIAN_POINT('Ctrl Pts',(178.414598463368,6.07188520349623,-107.928219936917));
#18875=CARTESIAN_POINT('Ctrl Pts',(178.415213505117,6.07361723123663,-107.928366463213));
#18876=CARTESIAN_POINT('Ctrl Pts',(178.415890038074,6.07552244369575,-107.928526920857));
#18877=CARTESIAN_POINT('Ctrl Pts',(178.416671529666,6.07772300303662,-107.928710903972));
#18878=CARTESIAN_POINT('Ctrl Pts',(178.417481884439,6.0800048366274,-107.928901682219));
#18879=CARTESIAN_POINT('Ctrl Pts',(178.418405026846,6.08260404766235,-107.929117745108));
#18880=CARTESIAN_POINT('Ctrl Pts',(178.419469997538,6.08560145625783,-107.929364432221));
#18881=CARTESIAN_POINT('Ctrl Pts',(178.420583048303,6.0887341884148,-107.92962225648));
#18882=CARTESIAN_POINT('Ctrl Pts',(178.421850942572,6.09230165151869,-107.929913509125));
#18883=CARTESIAN_POINT('Ctrl Pts',(178.423287109935,6.09633987574133,-107.930238780429));
#18884=CARTESIAN_POINT('Ctrl Pts',(178.424806597946,6.10061238147632,-107.930582922664));
#18885=CARTESIAN_POINT('Ctrl Pts',(178.426514350532,6.10541155145395,-107.930965095528));
#18886=CARTESIAN_POINT('Ctrl Pts',(178.428406024718,6.11072251269353,-107.931380513992));
#18887=CARTESIAN_POINT('Ctrl Pts',(178.430450932505,6.11646368422914,-107.931829583108));
#18888=CARTESIAN_POINT('Ctrl Pts',(178.43271062602,6.12280247841158,-107.932317405234));
#18889=CARTESIAN_POINT('Ctrl Pts',(178.435158382966,6.1296602790685,-107.932832831001));
#18890=CARTESIAN_POINT('Ctrl Pts',(178.437934870285,6.13743907287411,-107.933417477737));
#18891=CARTESIAN_POINT('Ctrl Pts',(178.440953077155,6.14588483863718,-107.93403743716));
#18892=CARTESIAN_POINT('Ctrl Pts',(178.444150457434,6.15481772739735,-107.934672492242));
#18893=CARTESIAN_POINT('Ctrl Pts',(178.449103370998,6.16865525126056,-107.93565622663));
#18894=CARTESIAN_POINT('Ctrl Pts',(178.454484757555,6.18365673275744,-107.936674546861));
#18895=CARTESIAN_POINT('Ctrl Pts',(178.460013146549,6.19902659477107,-107.937657083293));
#18896=CARTESIAN_POINT('Ctrl Pts',(178.463544791462,6.20884516850738,-107.938284747119));
#18897=CARTESIAN_POINT('Ctrl Pts',(178.467135303381,6.21881124737588,-107.938898064687));
#18898=CARTESIAN_POINT('Ctrl Pts',(178.47071856603,6.2287406065041,-107.939484838886));
#18899=CARTESIAN_POINT('Ctrl Pts',(178.474077874763,6.23804938068681,-107.940034939697));
#18900=CARTESIAN_POINT('Ctrl Pts',(178.477430296671,6.24732450793906,-107.940561734482));
#18901=CARTESIAN_POINT('Ctrl Pts',(178.480737796232,6.25646134033518,-107.94106038123));
#18902=CARTESIAN_POINT('Ctrl Pts',(178.483628027253,6.26444548543807,-107.94149611955));
#18903=CARTESIAN_POINT('Ctrl Pts',(178.486483935739,6.27232401612018,-107.94191045257));
#18904=CARTESIAN_POINT('Ctrl Pts',(178.489295938703,6.28007146975104,-107.94230335782));
#18905=CARTESIAN_POINT('Ctrl Pts',(178.49193892756,6.28735326634753,-107.942672647685));
#18906=CARTESIAN_POINT('Ctrl Pts',(178.49454303769,6.29451903346483,-107.943023052383));
#18907=CARTESIAN_POINT('Ctrl Pts',(178.497116199141,6.30159180694569,-107.94335674417));
#18908=CARTESIAN_POINT('Ctrl Pts',(178.499585573981,6.30837930520869,-107.943676976741));
#18909=CARTESIAN_POINT('Ctrl Pts',(178.502026355481,6.31508092194477,-107.94398185317));
#18910=CARTESIAN_POINT('Ctrl Pts',(178.504461997836,6.32176249687495,-107.944274820287));
#18911=CARTESIAN_POINT('Ctrl Pts',(178.506947342092,6.32858041652259,-107.944573765714));
#18912=CARTESIAN_POINT('Ctrl Pts',(178.509430123365,6.33538518866083,-107.944860667827));
#18913=CARTESIAN_POINT('Ctrl Pts',(178.511941391018,6.34226352759025,-107.94513878121));
#18914=CARTESIAN_POINT('Ctrl Pts',(178.514532849449,6.34936150832142,-107.945425775418));
#18915=CARTESIAN_POINT('Ctrl Pts',(178.51715458036,6.35653763787409,-107.94570334598));
#18916=CARTESIAN_POINT('Ctrl Pts',(178.519820335973,6.36383079184547,-107.94597187229));
#18917=CARTESIAN_POINT('Ctrl Pts',(178.522634229987,6.37152923284386,-107.946255320844));
#18918=CARTESIAN_POINT('Ctrl Pts',(178.525497070125,6.37935775149736,-107.946528613934));
#18919=CARTESIAN_POINT('Ctrl Pts',(178.528404154866,6.3873045340961,-107.946789831109));
#18920=CARTESIAN_POINT('Ctrl Pts',(178.531532994176,6.39585750313594,-107.947070974124));
#18921=CARTESIAN_POINT('Ctrl Pts',(178.53471292725,6.40454701494677,-107.947338023315));
#18922=CARTESIAN_POINT('Ctrl Pts',(178.537916535956,6.41329921114082,-107.947587389251));
#18923=CARTESIAN_POINT('Ctrl Pts',(178.541525048346,6.42315759626256,-107.947868272515));
#18924=CARTESIAN_POINT('Ctrl Pts',(178.545163323259,6.43309474441174,-107.948126551975));
#18925=CARTESIAN_POINT('Ctrl Pts',(178.54876895076,6.44294166046983,-107.948357926994));
#18926=CARTESIAN_POINT('Ctrl Pts',(178.555559818195,6.46148742028091,-107.948793700539));
#18927=CARTESIAN_POINT('Ctrl Pts',(178.562232479394,6.47970668810108,-107.949130963775));
#18928=CARTESIAN_POINT('Ctrl Pts',(178.56828435694,6.49623651029247,-107.949371076525));
#18929=CARTESIAN_POINT('Ctrl Pts',(178.571379491104,6.50469041852403,-107.949493878279));
#18930=CARTESIAN_POINT('Ctrl Pts',(178.5743116503,6.51270076910019,-107.949592066599));
#18931=CARTESIAN_POINT('Ctrl Pts',(178.577024251211,6.52011387104887,-107.949670003794));
#18932=CARTESIAN_POINT('Ctrl Pts',(178.579468755426,6.52679430784969,-107.949740238159));
#18933=CARTESIAN_POINT('Ctrl Pts',(178.581734724378,6.53298908286734,-107.949794115064));
#18934=CARTESIAN_POINT('Ctrl Pts',(178.583795074241,6.53862447881607,-107.949835858399));
#18935=CARTESIAN_POINT('Ctrl Pts',(178.585722016495,6.54389498299908,-107.949874898855));
#18936=CARTESIAN_POINT('Ctrl Pts',(178.587468955848,6.54867578942129,-107.949903374666));
#18937=CARTESIAN_POINT('Ctrl Pts',(178.589029536264,6.55294946252688,-107.949924777042));
#18938=CARTESIAN_POINT('Ctrl Pts',(178.590481114101,6.55692463041785,-107.949944684516));
#18939=CARTESIAN_POINT('Ctrl Pts',(178.591771416975,6.56046091966274,-107.949958491691));
#18940=CARTESIAN_POINT('Ctrl Pts',(178.592910673727,6.5635860256236,-107.949968587791));
#18941=CARTESIAN_POINT('Ctrl Pts',(178.594015383929,6.56661636661492,-107.94997837774));
#18942=CARTESIAN_POINT('Ctrl Pts',(178.594977967003,6.56925979976113,-107.949984684072));
#18943=CARTESIAN_POINT('Ctrl Pts',(178.595823866001,6.57158547788136,-107.949989099866));
#18944=CARTESIAN_POINT('Ctrl Pts',(178.596647541579,6.57385005588911,-107.949993399649));
#18945=CARTESIAN_POINT('Ctrl Pts',(178.597360497027,6.57581311704121,-107.949995903734));
#18946=CARTESIAN_POINT('Ctrl Pts',(178.598003120442,6.57758458484291,-107.949997507791));
#18947=CARTESIAN_POINT('Ctrl Pts',(178.598625651554,6.57930066582568,-107.949999061696));
#18948=CARTESIAN_POINT('Ctrl Pts',(178.599182131485,6.5808368133178,-107.949999767001));
#18949=CARTESIAN_POINT('Ctrl Pts',(178.599726292418,6.58233938722526,-107.949999953178));
#18950=CARTESIAN_POINT('Ctrl Pts',(178.599817733258,6.58259187984708,-107.949999984463));
#18951=CARTESIAN_POINT('Ctrl Pts',(178.599908867259,6.58284353638597,-107.95));
#18952=CARTESIAN_POINT('Ctrl Pts',(178.6,6.58309518948451,-107.95));
#18953=CARTESIAN_POINT('',(178.706458129484,6.29154759474225,-107.95));
#18954=CARTESIAN_POINT('Ctrl Pts',(178.412949234542,6.06724049855578,-107.927825180321));
#18955=CARTESIAN_POINT('Ctrl Pts',(178.240471965366,5.58142596856032,-107.886347987194));
#18956=CARTESIAN_POINT('Ctrl Pts',(178.066773026242,5.05523969179933,-107.780573504214));
#18957=CARTESIAN_POINT('Ctrl Pts',(177.858376158784,4.15716129915578,-107.487588730723));
#18958=CARTESIAN_POINT('Ctrl Pts',(177.799999999912,3.77824139277387,-107.327421746315));
#18959=CARTESIAN_POINT('Ctrl Pts',(177.8,3.42868316199151,-107.149999999604));
#18960=CARTESIAN_POINT('Ctrl Pts',(178.537807502978,6.02164757478294,-107.935082460943));
#18961=CARTESIAN_POINT('Ctrl Pts',(178.363767312538,5.53583597592066,-107.905551798508));
#18962=CARTESIAN_POINT('Ctrl Pts',(178.183613995588,5.01057297796046,-107.812220700977));
#18963=CARTESIAN_POINT('Ctrl Pts',(177.955395688911,4.11610793281407,-107.53590212866));
#18964=CARTESIAN_POINT('Ctrl Pts',(177.885823288832,3.73937765491853,-107.381196742299));
#18965=CARTESIAN_POINT('Ctrl Pts',(177.872973082299,3.39266652940119,-107.206172926527));
#18966=CARTESIAN_POINT('Ctrl Pts',(178.662665771413,5.97605465101009,-107.942339741564));
#18967=CARTESIAN_POINT('Ctrl Pts',(178.486832509378,5.49026482889952,-107.924762702489));
#18968=CARTESIAN_POINT('Ctrl Pts',(178.300397762631,4.96591073123605,-107.843861291125));
#18969=CARTESIAN_POINT('Ctrl Pts',(178.052417412725,4.07505247364037,-107.58421556635));
#18970=CARTESIAN_POINT('Ctrl Pts',(177.971553851954,3.70051482129146,-107.434941903923));
#18971=CARTESIAN_POINT('Ctrl Pts',(177.945946164598,3.35664989681088,-107.262345853449));
#18972=CARTESIAN_POINT('Ctrl Pts',(178.787524039848,5.93046172723724,-107.949597022186));
#18973=CARTESIAN_POINT('Ctrl Pts',(178.61012785655,5.44467483625986,-107.943966513803));
#18974=CARTESIAN_POINT('Ctrl Pts',(178.417238731978,4.92124401739719,-107.875508487888));
#18975=CARTESIAN_POINT('Ctrl Pts',(178.149436942852,4.03399910729865,-107.632528964287));
#18976=CARTESIAN_POINT('Ctrl Pts',(178.057377140874,3.66165108343612,-107.488716899907));
#18977=CARTESIAN_POINT('Ctrl Pts',(178.018919246896,3.32063326422056,-107.318518780371));
#18978=CARTESIAN_POINT('',(178.018919246896,3.32063326422068,-107.318518780371));
#18979=CARTESIAN_POINT('Ctrl Pts',(178.787524039848,5.93046172723724,-107.949597022186));
#18980=CARTESIAN_POINT('Ctrl Pts',(178.61012785655,5.44467483625986,-107.943966513803));
#18981=CARTESIAN_POINT('Ctrl Pts',(178.417238731978,4.92124401739719,-107.875508487888));
#18982=CARTESIAN_POINT('Ctrl Pts',(178.149436942852,4.03399910729865,-107.632528964287));
#18983=CARTESIAN_POINT('Ctrl Pts',(178.057377140874,3.66165108343612,-107.488716899907));
#18984=CARTESIAN_POINT('Ctrl Pts',(178.018919246896,3.32063326422056,-107.318518780371));
#18985=CARTESIAN_POINT('',(177.8,3.42868316190266,-107.14999999978));
#18986=CARTESIAN_POINT('',(178.018919246896,3.32063326422068,-107.318518780371));
#18987=CARTESIAN_POINT('Ctrl Pts',(177.8,3.42868316199151,-107.149999999604));
#18988=CARTESIAN_POINT('Ctrl Pts',(177.799999999912,3.77824139277387,-107.327421746315));
#18989=CARTESIAN_POINT('Ctrl Pts',(177.858376158784,4.15716129915578,-107.487588730723));
#18990=CARTESIAN_POINT('Ctrl Pts',(178.066773026242,5.05523969179933,-107.780573504214));
#18991=CARTESIAN_POINT('Ctrl Pts',(178.240471965366,5.58142596856032,-107.886347987194));
#18992=CARTESIAN_POINT('Ctrl Pts',(178.412949234542,6.06724049855578,-107.927825180321));
#18993=CARTESIAN_POINT('Origin',(177.9,6.00000000000001,-101.95));
#18994=CARTESIAN_POINT('',(177.8,3.10645162089483,-106.976666666667));
#18995=CARTESIAN_POINT('',(178.,3.00667409058086,-107.15));
#18996=CARTESIAN_POINT('',(177.8,3.10645162089483,-106.976666666667));
#18997=CARTESIAN_POINT('',(178.,0.800000000000001,-104.943325909419));
#18998=CARTESIAN_POINT('Origin',(178.,6.00000000000001,-101.95));
#18999=CARTESIAN_POINT('',(177.8,0.97333333333333,-104.843548379105));
#19000=CARTESIAN_POINT('',(178.,0.800000000000001,-104.943325909419));
#19001=CARTESIAN_POINT('Origin',(177.8,6.00000000000001,-101.95));
#19002=CARTESIAN_POINT('Ctrl Pts',(177.8,3.42868316199162,-107.149999999604));
#19003=CARTESIAN_POINT('Ctrl Pts',(177.8,3.31801931336447,-107.093831465749));
#19004=CARTESIAN_POINT('Ctrl Pts',(177.8,3.21069598181731,-107.036673848678));
#19005=CARTESIAN_POINT('Ctrl Pts',(177.8,3.10645162089484,-106.976666666667));
#19006=CARTESIAN_POINT('Ctrl Pts',(177.872973082299,3.39266652940131,-107.206172926527));
#19007=CARTESIAN_POINT('Ctrl Pts',(177.868914723125,3.28290392767113,-107.150766682816));
#19008=CARTESIAN_POINT('Ctrl Pts',(177.866666666667,3.17639835547358,-107.093853853762));
#19009=CARTESIAN_POINT('Ctrl Pts',(177.866666666667,3.07319244412352,-107.034444444444));
#19010=CARTESIAN_POINT('Ctrl Pts',(177.945946164598,3.35664989681099,-107.262345853449));
#19011=CARTESIAN_POINT('Ctrl Pts',(177.937829446251,3.24778854197779,-107.207701899883));
#19012=CARTESIAN_POINT('Ctrl Pts',(177.933333333333,3.14210072912985,-107.151033858845));
#19013=CARTESIAN_POINT('Ctrl Pts',(177.933333333333,3.0399332673522,-107.092222222222));
#19014=CARTESIAN_POINT('Ctrl Pts',(178.018919246896,3.32063326422067,-107.318518780371));
#19015=CARTESIAN_POINT('Ctrl Pts',(178.006744169376,3.21267315628445,-107.26463711695));
#19016=CARTESIAN_POINT('Ctrl Pts',(178.,3.10780310278612,-107.208213863928));
#19017=CARTESIAN_POINT('Ctrl Pts',(178.,3.00667409058087,-107.15));
#19018=CARTESIAN_POINT('Ctrl Pts',(177.8,3.10645162089484,-106.976666666667));
#19019=CARTESIAN_POINT('Ctrl Pts',(177.8,3.21069598181731,-107.036673848678));
#19020=CARTESIAN_POINT('Ctrl Pts',(177.8,3.31801931336447,-107.093831465749));
#19021=CARTESIAN_POINT('Ctrl Pts',(177.8,3.42868316199162,-107.149999999604));
#19022=CARTESIAN_POINT('Ctrl Pts',(178.018919246896,3.32063326422067,-107.318518780371));
#19023=CARTESIAN_POINT('Ctrl Pts',(178.006744169376,3.21267315628445,-107.26463711695));
#19024=CARTESIAN_POINT('Ctrl Pts',(178.,3.10780310278612,-107.208213863928));
#19025=CARTESIAN_POINT('Ctrl Pts',(178.,3.00667409058087,-107.15));
#19026=CARTESIAN_POINT('Ctrl Pts',(177.8,0.800000000395799,-104.521316838008));
#19027=CARTESIAN_POINT('Ctrl Pts',(177.799999999912,0.622578253685065,-104.171758607226));
#19028=CARTESIAN_POINT('Ctrl Pts',(177.858375951321,0.462411299210277,-103.79283930267));
#19029=CARTESIAN_POINT('Ctrl Pts',(178.066773083588,0.169426307367239,-102.894760003766));
#19030=CARTESIAN_POINT('Ctrl Pts',(178.240470897403,0.0636521521020384,
-102.368576933864));
#19031=CARTESIAN_POINT('Ctrl Pts',(178.412949735578,0.0221746991903157,
-101.882758090243));
#19032=CARTESIAN_POINT('Ctrl Pts',(177.872973082299,0.743827073473454,-104.557333470599));
#19033=CARTESIAN_POINT('Ctrl Pts',(177.885823288774,0.568803257717161,-104.210622345397));
#19034=CARTESIAN_POINT('Ctrl Pts',(177.955395481534,0.414097901249308,-103.83389266854));
#19035=CARTESIAN_POINT('Ctrl Pts',(178.183614063642,0.137779119795014,-102.939426720499));
#19036=CARTESIAN_POINT('Ctrl Pts',(178.363766257608,0.0444483646880333,
-102.414166925692));
#19037=CARTESIAN_POINT('Ctrl Pts',(178.537808007848,0.014917453309238,-101.928351016583));
#19038=CARTESIAN_POINT('Ctrl Pts',(177.945946164598,0.687654146551109,-104.593350103189));
#19039=CARTESIAN_POINT('Ctrl Pts',(177.971553852012,0.515058096060438,-104.249485178393));
#19040=CARTESIAN_POINT('Ctrl Pts',(178.052417640032,0.36578440471743,-103.874946934064));
#19041=CARTESIAN_POINT('Ctrl Pts',(178.300397980669,0.106138520890286,-102.984088610155));
#19042=CARTESIAN_POINT('Ctrl Pts',(178.486834293191,0.0252371025851526,
-102.4597302221));
#19043=CARTESIAN_POINT('Ctrl Pts',(178.662666280119,0.00766020742816018,
-101.973943942923));
#19044=CARTESIAN_POINT('Ctrl Pts',(178.018919246896,0.631481219628764,-104.629366735779));
#19045=CARTESIAN_POINT('Ctrl Pts',(178.057377140874,0.461283100092534,-104.288348916564));
#19046=CARTESIAN_POINT('Ctrl Pts',(178.149437170246,0.317471006756462,-103.916000299934));
#19047=CARTESIAN_POINT('Ctrl Pts',(178.417238960723,0.0744913333180605,
-103.028755326887));
#19048=CARTESIAN_POINT('Ctrl Pts',(178.610129653397,0.0060333151711475,
-102.505320213928));
#19049=CARTESIAN_POINT('Ctrl Pts',(178.787524552389,0.000402961547082414,
-102.019536869264));
#19050=CARTESIAN_POINT('',(177.8,0.800000000220451,-104.521316838097));
#19051=CARTESIAN_POINT('Ctrl Pts',(178.412949735578,0.0221746991903157,
-101.882758090243));
#19052=CARTESIAN_POINT('Ctrl Pts',(178.240470897403,0.0636521521020384,
-102.368576933864));
#19053=CARTESIAN_POINT('Ctrl Pts',(178.066773083588,0.169426307367239,-102.894760003766));
#19054=CARTESIAN_POINT('Ctrl Pts',(177.858375951321,0.462411299210277,-103.79283930267));
#19055=CARTESIAN_POINT('Ctrl Pts',(177.799999999912,0.622578253685065,-104.171758607226));
#19056=CARTESIAN_POINT('Ctrl Pts',(177.8,0.800000000395799,-104.521316838008));
#19057=CARTESIAN_POINT('',(178.018919246896,0.631481219628702,-104.629366735779));
#19058=CARTESIAN_POINT('',(177.8,0.800000000220451,-104.521316838097));
#19059=CARTESIAN_POINT('Ctrl Pts',(178.018919246896,0.631481219628764,-104.629366735779));
#19060=CARTESIAN_POINT('Ctrl Pts',(178.057377140874,0.461283100092534,-104.288348916564));
#19061=CARTESIAN_POINT('Ctrl Pts',(178.149437170246,0.317471006756462,-103.916000299934));
#19062=CARTESIAN_POINT('Ctrl Pts',(178.417238960723,0.0744913333180605,
-103.028755326887));
#19063=CARTESIAN_POINT('Ctrl Pts',(178.610129653397,0.0060333151711475,
-102.505320213928));
#19064=CARTESIAN_POINT('Ctrl Pts',(178.787524552389,0.000402961547082414,
-102.019536869264));
#19065=CARTESIAN_POINT('Ctrl Pts',(177.8,0.973333333333337,-104.843548379105));
#19066=CARTESIAN_POINT('Ctrl Pts',(177.8,0.913326151321774,-104.739304018183));
#19067=CARTESIAN_POINT('Ctrl Pts',(177.8,0.856168534250961,-104.631980686636));
#19068=CARTESIAN_POINT('Ctrl Pts',(177.8,0.800000000395739,-104.521316838008));
#19069=CARTESIAN_POINT('Ctrl Pts',(177.866666666667,0.915555555555559,-104.876807555876));
#19070=CARTESIAN_POINT('Ctrl Pts',(177.866666666667,0.856146146238362,-104.773601644526));
#19071=CARTESIAN_POINT('Ctrl Pts',(177.868914723125,0.799233317184013,-104.667096072329));
#19072=CARTESIAN_POINT('Ctrl Pts',(177.872973082299,0.743827073473395,-104.557333470599));
#19073=CARTESIAN_POINT('Ctrl Pts',(177.933333333333,0.85777777777778,-104.910066732648));
#19074=CARTESIAN_POINT('Ctrl Pts',(177.933333333333,0.798966141154949,-104.80789927087));
#19075=CARTESIAN_POINT('Ctrl Pts',(177.937829446251,0.742298100117065,-104.702211458022));
#19076=CARTESIAN_POINT('Ctrl Pts',(177.945946164598,0.687654146551051,-104.593350103189));
#19077=CARTESIAN_POINT('Ctrl Pts',(178.,0.800000000000001,-104.943325909419));
#19078=CARTESIAN_POINT('Ctrl Pts',(178.,0.741786136071537,-104.842196897214));
#19079=CARTESIAN_POINT('Ctrl Pts',(178.006744169376,0.685362883050116,-104.737326843716));
#19080=CARTESIAN_POINT('Ctrl Pts',(178.018919246896,0.631481219628706,-104.629366735779));
#19081=CARTESIAN_POINT('Ctrl Pts',(177.8,0.800000000395739,-104.521316838008));
#19082=CARTESIAN_POINT('Ctrl Pts',(177.8,0.856168534250961,-104.631980686636));
#19083=CARTESIAN_POINT('Ctrl Pts',(177.8,0.913326151321774,-104.739304018183));
#19084=CARTESIAN_POINT('Ctrl Pts',(177.8,0.973333333333337,-104.843548379105));
#19085=CARTESIAN_POINT('Ctrl Pts',(178.,0.800000000000001,-104.943325909419));
#19086=CARTESIAN_POINT('Ctrl Pts',(178.,0.741786136071537,-104.842196897214));
#19087=CARTESIAN_POINT('Ctrl Pts',(178.006744169376,0.685362883050116,-104.737326843716));
#19088=CARTESIAN_POINT('Ctrl Pts',(178.018919246896,0.631481219628706,-104.629366735779));
#19089=CARTESIAN_POINT('Origin',(178.6,0.800000000000001,3.35000000000001));
#19090=CARTESIAN_POINT('',(178.6,5.55111512312578E-16,37.8669048105155));
#19091=CARTESIAN_POINT('',(178.6,0.,3.35000000000001));
#19092=CARTESIAN_POINT('',(178.412949235465,0.0221748194567917,38.3827594988839));
#19093=CARTESIAN_POINT('Ctrl Pts',(178.412949235466,0.0221748194567948,
38.3827594988839));
#19094=CARTESIAN_POINT('Ctrl Pts',(178.413479204254,0.0220473729950726,
38.3812667426025));
#19095=CARTESIAN_POINT('Ctrl Pts',(178.414010756786,0.0219200771046594,
38.3797698454647));
#19096=CARTESIAN_POINT('Ctrl Pts',(178.414598464366,0.0217800628456899,
38.3781147939891));
#19097=CARTESIAN_POINT('Ctrl Pts',(178.415213506154,0.0216335365404913,
38.3763827662698));
#19098=CARTESIAN_POINT('Ctrl Pts',(178.415890039171,0.021473078883751,38.3744775538397));
#19099=CARTESIAN_POINT('Ctrl Pts',(178.416671530857,0.0212890957475055,
38.372276994541));
#19100=CARTESIAN_POINT('Ctrl Pts',(178.417481885728,0.0210983174791605,
38.3699951609939));
#19101=CARTESIAN_POINT('Ctrl Pts',(178.418405028268,0.0208822545602319,
38.3673959500167));
#19102=CARTESIAN_POINT('Ctrl Pts',(178.419469999136,0.020635567408783,38.364398541496));
#19103=CARTESIAN_POINT('Ctrl Pts',(178.420583050087,0.0203777431090619,
38.3612658094169));
#19104=CARTESIAN_POINT('Ctrl Pts',(178.421850944588,0.0200864904140129,
38.3576983464094));
#19105=CARTESIAN_POINT('Ctrl Pts',(178.423287112231,0.0197612190513805,
38.3536601223018));
#19106=CARTESIAN_POINT('Ctrl Pts',(178.424806600538,0.0194170767537217,
38.349387616688));
#19107=CARTESIAN_POINT('Ctrl Pts',(178.426514353473,0.0190349038180035,
38.3445884468523));
#19108=CARTESIAN_POINT('Ctrl Pts',(178.428406028054,0.0186194852750736,
38.3392774857728));
#19109=CARTESIAN_POINT('Ctrl Pts',(178.430450936267,0.0181704160751999,
38.3335363144092));
#19110=CARTESIAN_POINT('Ctrl Pts',(178.432710630262,0.0176825938577037,
38.3271975204197));
#19111=CARTESIAN_POINT('Ctrl Pts',(178.435158387722,0.0171671679971481,
38.32033971997));
#19112=CARTESIAN_POINT('Ctrl Pts',(178.437934875626,0.016582521155743,38.3125609263962));
#19113=CARTESIAN_POINT('Ctrl Pts',(178.440953083125,0.015962561625803,38.3041151608828));
#19114=CARTESIAN_POINT('Ctrl Pts',(178.444150464042,0.0153275064450717,
38.2951822723775));
#19115=CARTESIAN_POINT('Ctrl Pts',(178.44910337839,0.0143437719454808,38.2813447494813));
#19116=CARTESIAN_POINT('Ctrl Pts',(178.454484765716,0.0133254516247874,
38.2663432690601));
#19117=CARTESIAN_POINT('Ctrl Pts',(178.460013155354,0.0123429151425505,
38.2509734080791));
#19118=CARTESIAN_POINT('Ctrl Pts',(178.463544800827,0.0117152512572958,
38.2411548345874));
#19119=CARTESIAN_POINT('Ctrl Pts',(178.467135313259,0.0111019336470022,
38.2311887559332));
#19120=CARTESIAN_POINT('Ctrl Pts',(178.47071857634,0.0105151594258905,38.2212593969797));
#19121=CARTESIAN_POINT('Ctrl Pts',(178.474077885478,0.00996505859359832,
38.2119506229607));
#19122=CARTESIAN_POINT('Ctrl Pts',(178.477430307718,0.00943826380387005,
38.2026754958373));
#19123=CARTESIAN_POINT('Ctrl Pts',(178.480737807519,0.00893961706793955,
38.1935386635314));
#19124=CARTESIAN_POINT('Ctrl Pts',(178.483628038754,0.00850387875849878,
38.1855545184929));
#19125=CARTESIAN_POINT('Ctrl Pts',(178.486483947384,0.00808954576042137,
38.1776759878461));
#19126=CARTESIAN_POINT('Ctrl Pts',(178.489295950413,0.00769664054413144,
38.1699285342222));
#19127=CARTESIAN_POINT('Ctrl Pts',(178.491938939309,0.00732735071308687,
38.1626467376943));
#19128=CARTESIAN_POINT('Ctrl Pts',(178.494543049409,0.00697694605925282,
38.1554809706184));
#19129=CARTESIAN_POINT('Ctrl Pts',(178.497116210763,0.00664325432236268,
38.1484081971558));
#19130=CARTESIAN_POINT('Ctrl Pts',(178.499585585533,0.00632302179792544,
38.1416206988443));
#19131=CARTESIAN_POINT('Ctrl Pts',(178.502026366902,0.00601814542141101,
38.1349190820401));
#19132=CARTESIAN_POINT('Ctrl Pts',(178.504462009072,0.00572517836110786,
38.1282375070276));
#19133=CARTESIAN_POINT('Ctrl Pts',(178.506947353139,0.00542623299299849,
38.1214195872942));
#19134=CARTESIAN_POINT('Ctrl Pts',(178.509430134168,0.00513933094283238,
38.1146148150562));
#19135=CARTESIAN_POINT('Ctrl Pts',(178.511941401537,0.00486121762499003,
38.107736476015));
#19136=CARTESIAN_POINT('Ctrl Pts',(178.514532859657,0.00457422348627795,
38.10063849522));
#19137=CARTESIAN_POINT('Ctrl Pts',(178.517154590214,0.00429665299515969,
38.0934623655918));
#19138=CARTESIAN_POINT('Ctrl Pts',(178.519820345447,0.00402812675590003,
38.0861692115369));
#19139=CARTESIAN_POINT('Ctrl Pts',(178.522634239058,0.0037446782757912,
38.0784707704542));
#19140=CARTESIAN_POINT('Ctrl Pts',(178.525497078762,0.0034713852594164,
38.0706422517076));
#19141=CARTESIAN_POINT('Ctrl Pts',(178.528404163057,0.00321016815445696,
38.0626954690102));
#19142=CARTESIAN_POINT('Ctrl Pts',(178.531533001884,0.00292902521621764,
38.0541424998719));
#19143=CARTESIAN_POINT('Ctrl Pts',(178.534712934459,0.00266197609671292,
38.0454529879565));
#19144=CARTESIAN_POINT('Ctrl Pts',(178.537916542669,0.00241261022643413,
38.0367007916547));
#19145=CARTESIAN_POINT('Ctrl Pts',(178.541525054487,0.00213172703747435,
38.0268424064438));
#19146=CARTESIAN_POINT('Ctrl Pts',(178.54516332883,0.0018734476443256,38.0169052582021));
#19147=CARTESIAN_POINT('Ctrl Pts',(178.548768955785,0.00164207268377403,
38.0070583420493));
#19148=CARTESIAN_POINT('Ctrl Pts',(178.555559822268,0.00120629924286804,
37.9885125818511));
#19149=CARTESIAN_POINT('Ctrl Pts',(178.562232482599,0.000869036079380652,
37.9702933136435));
#19150=CARTESIAN_POINT('Ctrl Pts',(178.568284359434,0.000628923375684654,
37.9537634911092));
#19151=CARTESIAN_POINT('Ctrl Pts',(178.571379493236,0.000506121645651807,
37.9453095827024));
#19152=CARTESIAN_POINT('Ctrl Pts',(178.574311652108,0.00040793334416573,
37.9372992319626));
#19153=CARTESIAN_POINT('Ctrl Pts',(178.577024252739,0.000329996162289015,
37.9298861298665));
#19154=CARTESIAN_POINT('Ctrl Pts',(178.579468756696,0.000259761809582353,
37.9232056929462));
#19155=CARTESIAN_POINT('Ctrl Pts',(178.581734725427,0.000205884912835238,
37.9170109178203));
#19156=CARTESIAN_POINT('Ctrl Pts',(178.583795075103,0.000164141583355315,
37.9113755217763));
#19157=CARTESIAN_POINT('Ctrl Pts',(178.585722017181,0.000125101133586624,
37.9061050175084));
#19158=CARTESIAN_POINT('Ctrl Pts',(178.587468956389,9.66253259402746E-5,
37.9013242110118));
#19159=CARTESIAN_POINT('Ctrl Pts',(178.589029536688,7.5222952356846E-5,
37.897050537843));
#19160=CARTESIAN_POINT('Ctrl Pts',(178.590481114415,5.53154802371808E-5,
37.893075369896));
#19161=CARTESIAN_POINT('Ctrl Pts',(178.591771417204,4.15083062714315E-5,
37.8895390806041));
#19162=CARTESIAN_POINT('Ctrl Pts',(178.592910673892,3.1412207123438E-5,
37.886413974605));
#19163=CARTESIAN_POINT('Ctrl Pts',(178.59401538403,2.16222596854959E-5,
37.8833836335772));
#19164=CARTESIAN_POINT('Ctrl Pts',(178.59497796706,1.53159280371486E-5,
37.8807402004026));
#19165=CARTESIAN_POINT('Ctrl Pts',(178.595823866029,1.09001335970582E-5,
37.8784145222615));
#19166=CARTESIAN_POINT('Ctrl Pts',(178.596647541578,6.6003507133465E-6,
37.8761499442337));
#19167=CARTESIAN_POINT('Ctrl Pts',(178.597360497011,4.09626587143205E-6,
37.8741868830685));
#19168=CARTESIAN_POINT('Ctrl Pts',(178.598003120417,2.49220892567514E-6,
37.8724154152598));
#19169=CARTESIAN_POINT('Ctrl Pts',(178.598625651521,9.38304521417067E-7,
37.8706993342708));
#19170=CARTESIAN_POINT('Ctrl Pts',(178.59918213145,2.32998665909085E-7,
37.8691631867779));
#19171=CARTESIAN_POINT('Ctrl Pts',(178.599726292382,4.68224145011575E-8,
37.867660612874));
#19172=CARTESIAN_POINT('Ctrl Pts',(178.599817733235,1.55373403223607E-8,
37.8674081202189));
#19173=CARTESIAN_POINT('Ctrl Pts',(178.599908867247,6.6612116756507E-16,
37.867156463647));
#19174=CARTESIAN_POINT('Ctrl Pts',(178.6,6.66133814775094E-16,37.8669048105155));
#19175=CARTESIAN_POINT('',(177.8,0.800000000220449,41.0213168380973));
#19176=CARTESIAN_POINT('Ctrl Pts',(177.8,0.800000000395797,41.0213168380085));
#19177=CARTESIAN_POINT('Ctrl Pts',(177.799999999912,0.62257825368506,40.6717586072261));
#19178=CARTESIAN_POINT('Ctrl Pts',(177.858376073723,0.4624110846645,40.2928391623376));
#19179=CARTESIAN_POINT('Ctrl Pts',(178.066773051231,0.169426085453293,39.3947605243754));
#19180=CARTESIAN_POINT('Ctrl Pts',(178.240471017511,0.0636522405289915,
38.8685766805066));
#19181=CARTESIAN_POINT('Ctrl Pts',(178.412949235465,0.0221748194567911,
38.3827594988839));
#19182=CARTESIAN_POINT('',(177.8,0.800000000000001,3.35000000000001));
#19183=CARTESIAN_POINT('Origin',(177.8,0.,38.45));
#19184=CARTESIAN_POINT('',(181.549583741031,0.,-101.95));
#19185=CARTESIAN_POINT('',(177.8,0.,-101.95));
#19186=CARTESIAN_POINT('',(181.7625,5.55111512312578E-16,-101.366904810515));
#19187=CARTESIAN_POINT('',(181.656041870516,2.77555756156289E-16,-101.658452405258));
#19188=CARTESIAN_POINT('',(181.7625,5.55111512312578E-16,37.8669048105155));
#19189=CARTESIAN_POINT('',(181.7625,0.,3.35000000000001));
#19190=CARTESIAN_POINT('',(181.549583741031,2.22044604925031E-15,38.45));
#19191=CARTESIAN_POINT('',(181.656041870515,1.38777878078145E-15,38.1584524052577));
#19192=CARTESIAN_POINT('',(178.812916258969,2.22044604925031E-15,38.45));
#19193=CARTESIAN_POINT('',(177.8,2.22044604925031E-15,38.45));
#19194=CARTESIAN_POINT('',(178.706458129484,1.38777878078145E-15,38.1584524052578));
#19195=CARTESIAN_POINT('Origin',(177.8,6.00000000000001,-101.95));
#19196=CARTESIAN_POINT('',(181.549583741031,6.,-107.95));
#19197=CARTESIAN_POINT('',(177.8,6.,-107.95));
#19198=CARTESIAN_POINT('',(181.574975446846,5.93046313286183,-107.949597038478));
#19199=CARTESIAN_POINT('Ctrl Pts',(181.574975446847,5.93046313286183,-107.949597038478));
#19200=CARTESIAN_POINT('Ctrl Pts',(181.574851587102,5.93080231399545,-107.949600969674));
#19201=CARTESIAN_POINT('Ctrl Pts',(181.574726118725,5.93114590045353,-107.949604929021));
#19202=CARTESIAN_POINT('Ctrl Pts',(181.574566383937,5.93158332281071,-107.949609917176));
#19203=CARTESIAN_POINT('Ctrl Pts',(181.574399215445,5.93204110183877,-107.949615137469));
#19204=CARTESIAN_POINT('Ctrl Pts',(181.574194656871,5.93260127070279,-107.949621481053));
#19205=CARTESIAN_POINT('Ctrl Pts',(181.573935264898,5.93331159796672,-107.949629376639));
#19206=CARTESIAN_POINT('Ctrl Pts',(181.573641850187,5.93411509418438,-107.949638307838));
#19207=CARTESIAN_POINT('Ctrl Pts',(181.573278283541,5.93511069786036,-107.949649222747));
#19208=CARTESIAN_POINT('Ctrl Pts',(181.572843534142,5.93630123568595,-107.949661862757));
#19209=CARTESIAN_POINT('Ctrl Pts',(181.5723678608,5.93760384152415,-107.9496756926));
#19210=CARTESIAN_POINT('Ctrl Pts',(181.571807418754,5.9391385869165,-107.94969155866));
#19211=CARTESIAN_POINT('Ctrl Pts',(181.571184449722,5.94084456975789,-107.949708379169));
#19212=CARTESIAN_POINT('Ctrl Pts',(181.570252774797,5.94339593483727,-107.949733534908));
#19213=CARTESIAN_POINT('Ctrl Pts',(181.569182929476,5.94632569724474,-107.949760665181));
#19214=CARTESIAN_POINT('Ctrl Pts',(181.568089299526,5.94932062429873,-107.949785962922));
#19215=CARTESIAN_POINT('Ctrl Pts',(181.567351775576,5.95134034809351,-107.949803023254));
#19216=CARTESIAN_POINT('Ctrl Pts',(181.566604545459,5.95338666560009,-107.949819263662));
#19217=CARTESIAN_POINT('Ctrl Pts',(181.565874294746,5.95538649749657,-107.94983413399));
#19218=CARTESIAN_POINT('Ctrl Pts',(181.565237964273,5.95712912362859,-107.949847091791));
#19219=CARTESIAN_POINT('Ctrl Pts',(181.564614768374,5.95883579007666,-107.949859020331));
#19220=CARTESIAN_POINT('Ctrl Pts',(181.564008582509,5.96049588210055,-107.949869950646));
#19221=CARTESIAN_POINT('Ctrl Pts',(181.563441613107,5.96204857647315,-107.949880173838));
#19222=CARTESIAN_POINT('Ctrl Pts',(181.562889712943,5.96356001028182,-107.949889531659));
#19223=CARTESIAN_POINT('Ctrl Pts',(181.56234018139,5.9650649629533,-107.949898294404));
#19224=CARTESIAN_POINT('Ctrl Pts',(181.5617897477,5.96657238622942,-107.949907071534));
#19225=CARTESIAN_POINT('Ctrl Pts',(181.561238593153,5.9680817889974,-107.949915301922));
#19226=CARTESIAN_POINT('Ctrl Pts',(181.560672630617,5.96963174796805,-107.949923146947));
#19227=CARTESIAN_POINT('Ctrl Pts',(181.56005990152,5.97130978299697,-107.949931640221));
#19228=CARTESIAN_POINT('Ctrl Pts',(181.55942999806,5.97303485537968,-107.949939665741));
#19229=CARTESIAN_POINT('Ctrl Pts',(181.55878590025,5.97479880212237,-107.949947074735));
#19230=CARTESIAN_POINT('Ctrl Pts',(181.558033049521,5.97686058306593,-107.949955734703));
#19231=CARTESIAN_POINT('Ctrl Pts',(181.557261103323,5.97897466126266,-107.949963524226));
#19232=CARTESIAN_POINT('Ctrl Pts',(181.55649893061,5.98106197314285,-107.94997011252));
#19233=CARTESIAN_POINT('Ctrl Pts',(181.555584005774,5.98356761713471,-107.949978021219));
#19234=CARTESIAN_POINT('Ctrl Pts',(181.554684783888,5.98603025599236,-107.949984153345));
#19235=CARTESIAN_POINT('Ctrl Pts',(181.553868772039,5.98826500948326,-107.949988524155));
#19236=CARTESIAN_POINT('Ctrl Pts',(181.553239803013,5.98998752212496,-107.949991893107));
#19237=CARTESIAN_POINT('Ctrl Pts',(181.552661056841,5.99157249064165,-107.949994240505));
#19238=CARTESIAN_POINT('Ctrl Pts',(181.552156544722,5.99295415655168,-107.949995863006));
#19239=CARTESIAN_POINT('Ctrl Pts',(181.551698261038,5.99420922044089,-107.949997336838));
#19240=CARTESIAN_POINT('Ctrl Pts',(181.551301549687,5.99529565802532,-107.949998223794));
#19241=CARTESIAN_POINT('Ctrl Pts',(181.550971624754,5.99619919007983,-107.949998796154));
#19242=CARTESIAN_POINT('Ctrl Pts',(181.550662042814,5.99704701083767,-107.949999333221));
#19243=CARTESIAN_POINT('Ctrl Pts',(181.550411466451,5.9977332351975,-107.94999959747));
#19244=CARTESIAN_POINT('Ctrl Pts',(181.550208860189,5.99828808589276,-107.949999755779));
#19245=CARTESIAN_POINT('Ctrl Pts',(181.550019269662,5.99880729213513,-107.949999903919));
#19246=CARTESIAN_POINT('Ctrl Pts',(181.549871769533,5.9992112272231,-107.949999958751));
#19247=CARTESIAN_POINT('Ctrl Pts',(181.549741547127,5.99956784464628,-107.949999984437));
#19248=CARTESIAN_POINT('Ctrl Pts',(181.549687047567,5.99971709310156,-107.949999995187));
#19249=CARTESIAN_POINT('Ctrl Pts',(181.549635368945,5.99985861598446,-107.95));
#19250=CARTESIAN_POINT('Ctrl Pts',(181.549583741031,6.,-107.95));
#19251=CARTESIAN_POINT('',(182.343580753104,3.32063326422071,-107.318518780371));
#19252=CARTESIAN_POINT('Ctrl Pts',(182.343580753104,3.32063326422059,-107.318518780371));
#19253=CARTESIAN_POINT('Ctrl Pts',(182.305122859126,3.66165108343612,-107.488716899907));
#19254=CARTESIAN_POINT('Ctrl Pts',(182.21306296514,4.03399937391406,-107.632528959141));
#19255=CARTESIAN_POINT('Ctrl Pts',(181.945261097542,4.92124458677734,-107.875508608848));
#19256=CARTESIAN_POINT('Ctrl Pts',(181.752371143193,5.4446775876699,-107.943966659521));
#19257=CARTESIAN_POINT('Ctrl Pts',(181.574975446846,5.93046313286183,-107.949597038478));
#19258=CARTESIAN_POINT('',(182.3625,3.00667409058086,-107.15));
#19259=CARTESIAN_POINT('Ctrl Pts',(182.3625,3.00667409058087,-107.15));
#19260=CARTESIAN_POINT('Ctrl Pts',(182.3625,3.10780310278612,-107.208213863928));
#19261=CARTESIAN_POINT('Ctrl Pts',(182.355755830624,3.21267315628447,-107.26463711695));
#19262=CARTESIAN_POINT('Ctrl Pts',(182.343580753104,3.32063326422071,-107.318518780371));
#19263=CARTESIAN_POINT('',(182.3625,0.800000000000001,-104.943325909419));
#19264=CARTESIAN_POINT('Origin',(182.3625,6.00000000000001,-101.95));
#19265=CARTESIAN_POINT('',(182.343580753256,0.631481220303021,-104.62936673713));
#19266=CARTESIAN_POINT('Ctrl Pts',(182.343580753256,0.631481220303025,-104.62936673713));
#19267=CARTESIAN_POINT('Ctrl Pts',(182.355987338329,0.686387436939596,-104.739379693196));
#19268=CARTESIAN_POINT('Ctrl Pts',(182.3625,0.743322320630639,-104.844865554069));
#19269=CARTESIAN_POINT('Ctrl Pts',(182.3625,0.799999999999998,-104.943325909419));
#19270=CARTESIAN_POINT('',(181.5749753816,0.000402959451920593,-102.019536688494));
#19271=CARTESIAN_POINT('Ctrl Pts',(181.5749753816,0.000402959451920593,
-102.019536688494));
#19272=CARTESIAN_POINT('Ctrl Pts',(181.765769469498,0.0064585754895931,
-102.542012763284));
#19273=CARTESIAN_POINT('Ctrl Pts',(181.990548412461,0.0977146252752476,
-103.158388759139));
#19274=CARTESIAN_POINT('Ctrl Pts',(182.224838707103,0.341969925937946,-103.971322135667));
#19275=CARTESIAN_POINT('Ctrl Pts',(182.308539856551,0.47640526231532,-104.318648468817));
#19276=CARTESIAN_POINT('Ctrl Pts',(182.343580753256,0.631481220303202,-104.629366737131));
#19277=CARTESIAN_POINT('Ctrl Pts',(181.549583741031,0.,-101.95));
#19278=CARTESIAN_POINT('Ctrl Pts',(181.54970760812,0.,-101.950339212386));
#19279=CARTESIAN_POINT('Ctrl Pts',(181.549833083808,2.29071906254038E-8,
-101.950682830141));
#19280=CARTESIAN_POINT('Ctrl Pts',(181.549992825092,1.04587385862942E-7,
-101.951120289523));
#19281=CARTESIAN_POINT('Ctrl Pts',(181.550160000382,1.90068796205335E-7,
-101.951578107295));
#19282=CARTESIAN_POINT('Ctrl Pts',(181.550364564865,3.38981443109131E-7,
-101.952138321158));
#19283=CARTESIAN_POINT('Ctrl Pts',(181.550623961395,6.76258333776047E-7,
-101.952848701379));
#19284=CARTESIAN_POINT('Ctrl Pts',(181.550917381295,1.05777365854045E-6,
-101.953652257592));
#19285=CARTESIAN_POINT('Ctrl Pts',(181.551280951416,1.68214207260373E-6,
-101.954647931466));
#19286=CARTESIAN_POINT('Ctrl Pts',(181.551715702461,2.84071918610351E-6,
-101.955838546237));
#19287=CARTESIAN_POINT('Ctrl Pts',(181.552191377746,4.10835615815435E-6,
-101.957141236654));
#19288=CARTESIAN_POINT('Ctrl Pts',(181.552751819603,6.03030069600252E-6,
-101.958676074583));
#19289=CARTESIAN_POINT('Ctrl Pts',(181.553374786724,8.98242465474652E-6,
-101.960382148871));
#19290=CARTESIAN_POINT('Ctrl Pts',(181.554306457762,1.33974383844118E-5,
-101.962933647896));
#19291=CARTESIAN_POINT('Ctrl Pts',(181.555376295022,2.02235012763771E-5,
-101.965863539379));
#19292=CARTESIAN_POINT('Ctrl Pts',(181.556469915917,2.9637200332111E-5,
-101.968858566372));
#19293=CARTESIAN_POINT('Ctrl Pts',(181.557207433796,3.59856263709023E-5,
-101.970878357661));
#19294=CARTESIAN_POINT('Ctrl Pts',(181.557954657433,4.34621306637084E-5,
-101.97292472978));
#19295=CARTESIAN_POINT('Ctrl Pts',(181.558684902273,5.17698706108405E-5,
-101.974924601646));
#19296=CARTESIAN_POINT('Ctrl Pts',(181.559321227784,5.90091232076345E-5,
-101.97666726303));
#19297=CARTESIAN_POINT('Ctrl Pts',(181.559944419184,6.68608083979287E-5,
-101.978373953766));
#19298=CARTESIAN_POINT('Ctrl Pts',(181.560550601505,7.51708677384499E-5,
-101.980034060035));
#19299=CARTESIAN_POINT('Ctrl Pts',(181.561117567921,8.29433223074671E-5,
-101.98158676863));
#19300=CARTESIAN_POINT('Ctrl Pts',(181.561669465921,9.11028932043242E-5,
-101.983098207949));
#19301=CARTESIAN_POINT('Ctrl Pts',(181.562218996326,9.9782376472568E-5,
-101.984603158254));
#19302=CARTESIAN_POINT('Ctrl Pts',(181.562769428947,0.000108476109649939,
-101.986110579374));
#19303=CARTESIAN_POINT('Ctrl Pts',(181.56332058345,0.000117739478919532,
-101.987619972111));
#19304=CARTESIAN_POINT('Ctrl Pts',(181.563886546778,0.000127858198572639,
-101.989169912371));
#19305=CARTESIAN_POINT('Ctrl Pts',(181.564499277062,0.000138813053173701,
-101.990847928046));
#19306=CARTESIAN_POINT('Ctrl Pts',(181.565129182704,0.000150780753699223,
-101.992572970802));
#19307=CARTESIAN_POINT('Ctrl Pts',(181.56577328316,0.000163815454714999,
-101.994336876537));
#19308=CARTESIAN_POINT('Ctrl Pts',(181.566526137782,0.000179051020544146,
-101.99639861174));
#19309=CARTESIAN_POINT('Ctrl Pts',(181.567298088538,0.0001957630484375,
-101.998512628489));
#19310=CARTESIAN_POINT('Ctrl Pts',(181.568060265242,0.000213365986056147,
-102.0005998647));
#19311=CARTESIAN_POINT('Ctrl Pts',(181.568975191389,0.000234496765571556,
-102.003105408326));
#19312=CARTESIAN_POINT('Ctrl Pts',(181.569874413831,0.000256905535015469,
-102.005567926382));
#19313=CARTESIAN_POINT('Ctrl Pts',(181.57069042421,0.000278434394754612,
-102.007802553675));
#19314=CARTESIAN_POINT('Ctrl Pts',(181.571319393029,0.000295028523743357,
-102.009524971582));
#19315=CARTESIAN_POINT('Ctrl Pts',(181.571898137643,0.000311050051264457,
-102.011109842215));
#19316=CARTESIAN_POINT('Ctrl Pts',(181.572402646459,0.000325440246225384,
-102.012491415757));
#19317=CARTESIAN_POINT('Ctrl Pts',(181.572860927247,0.000338511870882684,
-102.013746396029));
#19318=CARTESIAN_POINT('Ctrl Pts',(181.57325763423,0.000350216032188715,
-102.014832754664));
#19319=CARTESIAN_POINT('Ctrl Pts',(181.573587553363,0.000360114993102734,
-102.015736217068));
#19320=CARTESIAN_POINT('Ctrl Pts',(181.573897129891,0.000369403590350718,
-102.016583972552));
#19321=CARTESIAN_POINT('Ctrl Pts',(181.574147699568,0.000377092172797711,
-102.017270139883));
#19322=CARTESIAN_POINT('Ctrl Pts',(181.574350298267,0.000383364144085796,
-102.017824942027));
#19323=CARTESIAN_POINT('Ctrl Pts',(181.574539881751,0.000389233195429729,
-102.018344102929));
#19324=CARTESIAN_POINT('Ctrl Pts',(181.574687374055,0.000393859622541619,
-102.01874800007));
#19325=CARTESIAN_POINT('Ctrl Pts',(181.574817588547,0.000397966817764051,
-102.019104583318));
#19326=CARTESIAN_POINT('Ctrl Pts',(181.574872083688,0.000399685690829952,
-102.019253814438));
#19327=CARTESIAN_POINT('Ctrl Pts',(181.574923757996,0.000401320969685316,
-102.019395320917));
#19328=CARTESIAN_POINT('Ctrl Pts',(181.5749753816,0.000402959451920815,
-102.019536688494));
#19329=CARTESIAN_POINT('Ctrl Pts',(178.412949792571,6.06724207026202,44.4278253145154));
#19330=CARTESIAN_POINT('Ctrl Pts',(178.42318867301,6.09608178690105,44.4302875443684));
#19331=CARTESIAN_POINT('Ctrl Pts',(178.514957272365,6.35253399018344,44.4503778941236));
#19332=CARTESIAN_POINT('Ctrl Pts',(178.592152189615,6.56142469489367,44.45));
#19333=CARTESIAN_POINT('Ctrl Pts',(178.6,6.58309518948451,44.45));
#19334=CARTESIAN_POINT('Ctrl Pts',(178.537808064946,6.02164914272028,44.4350825564341));
#19335=CARTESIAN_POINT('Ctrl Pts',(178.545154992406,6.04220443093549,44.4361237601754));
#19336=CARTESIAN_POINT('Ctrl Pts',(178.609869985354,6.22405274576398,44.452422433776));
#19337=CARTESIAN_POINT('Ctrl Pts',(178.665385913285,6.37331287412804,44.45));
#19338=CARTESIAN_POINT('Ctrl Pts',(178.670972086323,6.38873012632301,44.45));
#19339=CARTESIAN_POINT('Ctrl Pts',(178.662666337321,5.97605621517853,44.4423397983527));
#19340=CARTESIAN_POINT('Ctrl Pts',(178.667058000585,5.98825131680075,44.4425732795651));
#19341=CARTESIAN_POINT('Ctrl Pts',(178.706720690063,6.09746305536317,44.4476687386033));
#19342=CARTESIAN_POINT('Ctrl Pts',(178.738619636954,6.18520105336241,44.45));
#19343=CARTESIAN_POINT('Ctrl Pts',(178.741944172646,6.1943650631615,44.45));
#19344=CARTESIAN_POINT('Ctrl Pts',(178.787524609695,5.93046328763679,44.4495970402714));
#19345=CARTESIAN_POINT('Ctrl Pts',(178.788941720953,5.93434394615833,44.449642017998));
#19346=CARTESIAN_POINT('Ctrl Pts',(178.8015714622,5.96893024314017,44.4500079385574));
#19347=CARTESIAN_POINT('Ctrl Pts',(178.811853360624,5.99708923259677,44.45));
#19348=CARTESIAN_POINT('Ctrl Pts',(178.812916258969,6.,44.45));
#19349=CARTESIAN_POINT('',(178.6,6.58309518948451,44.45));
#19350=CARTESIAN_POINT('',(178.412949792571,6.06724207026202,44.4278253145154));
#19351=CARTESIAN_POINT('Ctrl Pts',(178.6,6.58309518948452,44.45));
#19352=CARTESIAN_POINT('Ctrl Pts',(178.599458517973,6.58159997199468,44.45));
#19353=CARTESIAN_POINT('Ctrl Pts',(178.598915520309,6.58010061762004,44.4499994906954));
#19354=CARTESIAN_POINT('Ctrl Pts',(178.598314514906,6.57844323223622,44.4499982244605));
#19355=CARTESIAN_POINT('Ctrl Pts',(178.597685564613,6.57670878356453,44.4499968993497));
#19356=CARTESIAN_POINT('Ctrl Pts',(178.596993094733,6.57480128952343,44.449994749902));
#19357=CARTESIAN_POINT('Ctrl Pts',(178.596192260443,6.57259867771452,44.4499909381484));
#19358=CARTESIAN_POINT('Ctrl Pts',(178.595361861441,6.57031475122541,44.4499869856747));
#19359=CARTESIAN_POINT('Ctrl Pts',(178.594415017345,6.56771370326992,44.4499812514669));
#19360=CARTESIAN_POINT('Ctrl Pts',(178.593322018501,6.56471476414272,44.4499721273664));
#19361=CARTESIAN_POINT('Ctrl Pts',(178.59217970018,6.561580503641,44.4499625915584));
#19362=CARTESIAN_POINT('Ctrl Pts',(178.590877823263,6.55801186637361,44.4499493490856));
#19363=CARTESIAN_POINT('Ctrl Pts',(178.589403093044,6.55397282717115,44.449929812898));
#19364=CARTESIAN_POINT('Ctrl Pts',(178.587842862039,6.54969961562671,44.4499091440561));
#19365=CARTESIAN_POINT('Ctrl Pts',(178.586089262768,6.54490018007633,44.4498814053308));
#19366=CARTESIAN_POINT('Ctrl Pts',(178.584147685166,6.53958934065723,44.4498429246511));
#19367=CARTESIAN_POINT('Ctrl Pts',(178.582048978208,6.53384870189507,44.4498013297799));
#19368=CARTESIAN_POINT('Ctrl Pts',(178.579730794754,6.52751097601296,44.4497471216981));
#19369=CARTESIAN_POINT('Ctrl Pts',(178.57722196257,6.52065463592149,44.449675659884));
#19370=CARTESIAN_POINT('Ctrl Pts',(178.574377026696,6.51287976440619,44.4495946244604));
#19371=CARTESIAN_POINT('Ctrl Pts',(178.571287228746,6.50443881327361,44.4494912617698));
#19372=CARTESIAN_POINT('Ctrl Pts',(178.56801862387,6.49551119955545,44.4493604891292));
#19373=CARTESIAN_POINT('Ctrl Pts',(178.56294420415,6.48165132329992,44.4491574681794));
#19374=CARTESIAN_POINT('Ctrl Pts',(178.557440622755,6.46662341589086,44.4488871027284));
#19375=CARTESIAN_POINT('Ctrl Pts',(178.551802564766,6.45122671631941,44.4485468096717));
#19376=CARTESIAN_POINT('Ctrl Pts',(178.548206420165,6.44140617915121,44.448329759219));
#19377=CARTESIAN_POINT('Ctrl Pts',(178.544556616115,6.43143843660386,44.4480847826414));
#19378=CARTESIAN_POINT('Ctrl Pts',(178.540921148225,6.4215076975126,44.4478155734711));
#19379=CARTESIAN_POINT('Ctrl Pts',(178.537512897078,6.41219762961454,44.4475631898739));
#19380=CARTESIAN_POINT('Ctrl Pts',(178.534117745962,6.40292145768546,44.4472896528906));
#19381=CARTESIAN_POINT('Ctrl Pts',(178.530774442786,6.39378380888695,44.4469992611216));
#19382=CARTESIAN_POINT('Ctrl Pts',(178.527853421831,6.38580030807624,44.4467455478335));
#19383=CARTESIAN_POINT('Ctrl Pts',(178.52497197727,6.3779225584153,44.4464790605755));
#19384=CARTESIAN_POINT('Ctrl Pts',(178.522139765614,6.37017599734817,44.4462020999102));
#19385=CARTESIAN_POINT('Ctrl Pts',(178.519478224497,6.36289624805762,44.4459418290378));
#19386=CARTESIAN_POINT('Ctrl Pts',(178.5168602412,6.35573258653662,44.445672374142));
#19387=CARTESIAN_POINT('Ctrl Pts',(178.514277799497,6.34866200275349,44.445394056013));
#19388=CARTESIAN_POINT('Ctrl Pts',(178.511798987803,6.34187515225487,44.4451269064267));
#19389=CARTESIAN_POINT('Ctrl Pts',(178.509353003695,6.33517429878812,44.4448516471374));
#19390=CARTESIAN_POINT('Ctrl Pts',(178.506916323581,6.328493643819,44.4445661893035));
#19391=CARTESIAN_POINT('Ctrl Pts',(178.504429011938,6.32167417219901,44.4442747999703));
#19392=CARTESIAN_POINT('Ctrl Pts',(178.5019486018,6.31486802670454,44.4439724785344));
#19393=CARTESIAN_POINT('Ctrl Pts',(178.499444072893,6.30798842616424,44.4436551552934));
#19394=CARTESIAN_POINT('Ctrl Pts',(178.496859698675,6.30088950140187,44.4433277156695));
#19395=CARTESIAN_POINT('Ctrl Pts',(178.494249717861,6.29371255464342,44.4429842542725));
#19396=CARTESIAN_POINT('Ctrl Pts',(178.491600486335,6.28641868903367,44.4426219435754));
#19397=CARTESIAN_POINT('Ctrl Pts',(178.488804030965,6.27871948666037,44.4422394984456));
#19398=CARTESIAN_POINT('Ctrl Pts',(178.485963962915,6.27089032428992,44.4418360005005));
#19399=CARTESIAN_POINT('Ctrl Pts',(178.483084978334,6.26294302810835,44.4414106883969));
#19400=CARTESIAN_POINT('Ctrl Pts',(178.479986370237,6.25438947194786,44.4409529313334));
#19401=CARTESIAN_POINT('Ctrl Pts',(178.476842858534,6.24569952323156,44.4404698404418));
#19402=CARTESIAN_POINT('Ctrl Pts',(178.473681436809,6.23694709174931,44.4399643160253));
#19403=CARTESIAN_POINT('Ctrl Pts',(178.470120305089,6.22708805866677,44.4393948763265));
#19404=CARTESIAN_POINT('Ctrl Pts',(178.466536752565,6.21715051315623,44.4387968743326));
#19405=CARTESIAN_POINT('Ctrl Pts',(178.46299166798,6.20730357410851,44.4381806372635));
#19406=CARTESIAN_POINT('Ctrl Pts',(178.456316782679,6.18876320161894,44.4370203513363));
#19407=CARTESIAN_POINT('Ctrl Pts',(178.44978125028,6.17055048437432,44.4357930266506));
#19408=CARTESIAN_POINT('Ctrl Pts',(178.443867806725,6.15402796694876,44.4346162999984));
#19409=CARTESIAN_POINT('Ctrl Pts',(178.440842493664,6.14557506005742,44.4340142875707));
#19410=CARTESIAN_POINT('Ctrl Pts',(178.437980411313,6.13756619273647,44.4334264231729));
#19411=CARTESIAN_POINT('Ctrl Pts',(178.435335029566,6.13015512599593,44.4328700067777));
#19412=CARTESIAN_POINT('Ctrl Pts',(178.432951184304,6.12347675666169,44.4323686006615));
#19413=CARTESIAN_POINT('Ctrl Pts',(178.430743513708,6.11728446376527,44.4318928704646));
#19414=CARTESIAN_POINT('Ctrl Pts',(178.428737104348,6.11165195374683,44.4314531467548));
#19415=CARTESIAN_POINT('Ctrl Pts',(178.42686063372,6.10638421535628,44.4310419003549));
#19416=CARTESIAN_POINT('Ctrl Pts',(178.425160333831,6.10160651578871,44.4306622290609));
#19417=CARTESIAN_POINT('Ctrl Pts',(178.423641481701,6.09733622922153,44.4303189559555));
#19418=CARTESIAN_POINT('Ctrl Pts',(178.422228714802,6.09336420364257,44.4299996589872));
#19419=CARTESIAN_POINT('Ctrl Pts',(178.420972968814,6.08983130045456,44.4297118814688));
#19420=CARTESIAN_POINT('Ctrl Pts',(178.419863784619,6.08670972753893,44.4294555432534));
#19421=CARTESIAN_POINT('Ctrl Pts',(178.418788240371,6.0836828273976,44.4292069794038));
#19422=CARTESIAN_POINT('Ctrl Pts',(178.417850600654,6.08104296971711,44.4289880063072));
#19423=CARTESIAN_POINT('Ctrl Pts',(178.417025912301,6.07872086557605,44.4287942496133));
#19424=CARTESIAN_POINT('Ctrl Pts',(178.416222893088,6.07645977599809,44.4286055839832));
#19425=CARTESIAN_POINT('Ctrl Pts',(178.415527051897,6.07450019982907,44.4284408442171));
#19426=CARTESIAN_POINT('Ctrl Pts',(178.414899175626,6.07273203935875,44.4282915166029));
#19427=CARTESIAN_POINT('Ctrl Pts',(178.41429092292,6.07101914074931,44.4281468560549));
#19428=CARTESIAN_POINT('Ctrl Pts',(178.413746500949,6.06948601365089,44.4280166669529));
#19429=CARTESIAN_POINT('Ctrl Pts',(178.413213947771,6.06798608491948,44.4278887906975));
#19430=CARTESIAN_POINT('Ctrl Pts',(178.413125702731,6.06773754397356,44.427867601367));
#19431=CARTESIAN_POINT('Ctrl Pts',(178.413037745286,6.06748980548983,44.4278464652458));
#19432=CARTESIAN_POINT('Ctrl Pts',(178.412949792571,6.06724207026203,44.4278253145154));
#19433=CARTESIAN_POINT('',(178.787524609695,5.93046328763679,44.4495970402714));
#19434=CARTESIAN_POINT('Ctrl Pts',(178.787524609695,5.93046328763679,44.4495970402714));
#19435=CARTESIAN_POINT('Ctrl Pts',(178.662666337321,5.97605621517853,44.4423397983527));
#19436=CARTESIAN_POINT('Ctrl Pts',(178.537808064946,6.02164914272028,44.4350825564341));
#19437=CARTESIAN_POINT('Ctrl Pts',(178.412949792571,6.06724207026202,44.4278253145154));
#19438=CARTESIAN_POINT('',(178.812916258969,6.,44.45));
#19439=CARTESIAN_POINT('Ctrl Pts',(178.787524609695,5.93046328763679,44.4495970402714));
#19440=CARTESIAN_POINT('Ctrl Pts',(178.787648469277,5.93080246830438,44.4496009714535));
#19441=CARTESIAN_POINT('Ctrl Pts',(178.787773937493,5.93114605429704,44.449604930787));
#19442=CARTESIAN_POINT('Ctrl Pts',(178.787933672098,5.93158347612988,44.4496099189249));
#19443=CARTESIAN_POINT('Ctrl Pts',(178.788100840397,5.93204125460652,44.4496151391996));
#19444=CARTESIAN_POINT('Ctrl Pts',(178.788305398756,5.9326014228527,44.4496214827624));
#19445=CARTESIAN_POINT('Ctrl Pts',(178.788564790463,5.9333117493612,44.4496293783222));
#19446=CARTESIAN_POINT('Ctrl Pts',(178.788858204901,5.93411524479927,44.4496383094914));
#19447=CARTESIAN_POINT('Ctrl Pts',(178.789221771224,5.93511084755497,44.4496492243657));
#19448=CARTESIAN_POINT('Ctrl Pts',(178.789656520216,5.93630138422979,44.4496618643344));
#19449=CARTESIAN_POINT('Ctrl Pts',(178.790132193253,5.93760398919225,44.449675694136));
#19450=CARTESIAN_POINT('Ctrl Pts',(178.790692634943,5.93913873356867,44.4496915601474));
#19451=CARTESIAN_POINT('Ctrl Pts',(178.791315603513,5.94084471510306,44.4497083806022));
#19452=CARTESIAN_POINT('Ctrl Pts',(178.792247276602,5.94339607509601,44.4497335362294));
#19453=CARTESIAN_POINT('Ctrl Pts',(178.793317119493,5.94632583079425,44.4497606663719));
#19454=CARTESIAN_POINT('Ctrl Pts',(178.794410746748,5.94932075042631,44.4497859639876));
#19455=CARTESIAN_POINT('Ctrl Pts',(178.795148269123,5.95134046987867,44.4498030242406));
#19456=CARTESIAN_POINT('Ctrl Pts',(178.795895497556,5.95338678275387,44.4498192645702));
#19457=CARTESIAN_POINT('Ctrl Pts',(178.796625746573,5.9553866099923,44.4498341348267));
#19458=CARTESIAN_POINT('Ctrl Pts',(178.797262075683,5.95712923238399,44.449847092567));
#19459=CARTESIAN_POINT('Ctrl Pts',(178.797885270207,5.95883589505943,44.4498590210502));
#19460=CARTESIAN_POINT('Ctrl Pts',(178.798491454741,5.96049598344251,44.4498699513136));
#19461=CARTESIAN_POINT('Ctrl Pts',(178.799058423271,5.96204867543337,44.4498801744635));
#19462=CARTESIAN_POINT('Ctrl Pts',(178.799610322583,5.96356010691652,44.4498895322452));
#19463=CARTESIAN_POINT('Ctrl Pts',(178.800159853383,5.96506505753999,44.4498982949543));
#19464=CARTESIAN_POINT('Ctrl Pts',(178.800710286014,5.96657247792421,44.4499070720438));
#19465=CARTESIAN_POINT('Ctrl Pts',(178.801261439609,5.96808187810208,44.4499153023956));
#19466=CARTESIAN_POINT('Ctrl Pts',(178.801827401211,5.96963183453364,44.449923147385));
#19467=CARTESIAN_POINT('Ctrl Pts',(178.802440129662,5.97130986781118,44.4499316406258));
#19468=CARTESIAN_POINT('Ctrl Pts',(178.803070032518,5.97303493856084,44.4499396661149));
#19469=CARTESIAN_POINT('Ctrl Pts',(178.803714129678,5.97479888354565,44.4499470750774));
#19470=CARTESIAN_POINT('Ctrl Pts',(178.804466980332,5.97686066430854,44.4499557350166));
#19471=CARTESIAN_POINT('Ctrl Pts',(178.805238926428,5.97897474224762,44.4499635245097));
#19472=CARTESIAN_POINT('Ctrl Pts',(178.806001098802,5.98106205322472,44.4499701127732));
#19473=CARTESIAN_POINT('Ctrl Pts',(178.806916020284,5.9835676880624,44.4499780214092));
#19474=CARTESIAN_POINT('Ctrl Pts',(178.807815238561,5.98603031706659,44.449984153484));
#19475=CARTESIAN_POINT('Ctrl Pts',(178.808631246937,5.98826506107557,44.4499885242564));
#19476=CARTESIAN_POINT('Ctrl Pts',(178.809260214051,5.98998756850614,44.4499918931828));
#19477=CARTESIAN_POINT('Ctrl Pts',(178.809838958277,5.99157253171875,44.4499942405612));
#19478=CARTESIAN_POINT('Ctrl Pts',(178.810343468533,5.99295419255149,44.4499958630484));
#19479=CARTESIAN_POINT('Ctrl Pts',(178.810801750615,5.99420925207889,44.4499973368673));
#19480=CARTESIAN_POINT('Ctrl Pts',(178.811198460408,5.99529568542398,44.4499982238154));
#19481=CARTESIAN_POINT('Ctrl Pts',(178.811528383922,5.99619921362319,44.4499987961685));
#19482=CARTESIAN_POINT('Ctrl Pts',(178.811837964558,5.99704703083499,44.4499993332306));
#19483=CARTESIAN_POINT('Ctrl Pts',(178.81208853973,5.99773325196068,44.4499995974758));
#19484=CARTESIAN_POINT('Ctrl Pts',(178.812291145002,5.99828809997737,44.4499997557832));
#19485=CARTESIAN_POINT('Ctrl Pts',(178.812480734631,5.99880730379097,44.4499999039207));
#19486=CARTESIAN_POINT('Ctrl Pts',(178.812628234028,5.99921123690189,44.4499999587523));
#19487=CARTESIAN_POINT('Ctrl Pts',(178.812758455955,5.99956785304632,44.4499999844374));
#19488=CARTESIAN_POINT('Ctrl Pts',(178.812812954392,5.99971709843905,44.4499999951867));
#19489=CARTESIAN_POINT('Ctrl Pts',(178.812864632032,5.99985861864849,44.45));
#19490=CARTESIAN_POINT('Ctrl Pts',(178.812916258969,6.,44.45));
#19491=CARTESIAN_POINT('',(178.706458129484,6.29154759474226,44.45));
#19492=CARTESIAN_POINT('Ctrl Pts',(178.787524038921,0.00040297784403398,
38.5195382753398));
#19493=CARTESIAN_POINT('Ctrl Pts',(178.788055467441,0.000386110442137109,
38.5180829960178));
#19494=CARTESIAN_POINT('Ctrl Pts',(178.789728852842,0.000327539963165485,
38.5135006260165));
#19495=CARTESIAN_POINT('Ctrl Pts',(178.796662726497,0.000156711167295762,
38.494512252932));
#19496=CARTESIAN_POINT('Ctrl Pts',(178.802273531769,5.97527433101154E-5,
38.4791464222591));
#19497=CARTESIAN_POINT('Ctrl Pts',(178.808321057158,7.82364703110596E-6,
38.4625844223785));
#19498=CARTESIAN_POINT('Ctrl Pts',(178.811886047181,-2.86362915729096E-7,
38.4528212764702));
#19499=CARTESIAN_POINT('Ctrl Pts',(178.81256195152,2.22118770383678E-15,
38.4509702776198));
#19500=CARTESIAN_POINT('Ctrl Pts',(178.812916258969,2.22044604925031E-15,
38.45));
#19501=CARTESIAN_POINT('Ctrl Pts',(178.662665771103,0.00766025838161988,
38.4739453498545));
#19502=CARTESIAN_POINT('Ctrl Pts',(178.664312652589,0.00757270116505651,
38.4693721648001));
#19503=CARTESIAN_POINT('Ctrl Pts',(178.670768458182,0.00689135909653072,
38.4515513889253));
#19504=CARTESIAN_POINT('Ctrl Pts',(178.689811944466,0.00496920533963629,
38.3991254694919));
#19505=CARTESIAN_POINT('Ctrl Pts',(178.709764883196,0.00276026299996931,
38.3441919684076));
#19506=CARTESIAN_POINT('Ctrl Pts',(178.727201211343,0.00110274141105337,
38.2962200342644));
#19507=CARTESIAN_POINT('Ctrl Pts',(178.737862157161,0.000211760193833221,
38.2668827645598));
#19508=CARTESIAN_POINT('Ctrl Pts',(178.740836000832,1.66580200687153E-15,
38.2586896296938));
#19509=CARTESIAN_POINT('Ctrl Pts',(178.741944172646,1.66533453693773E-15,
38.2556349368385));
#19510=CARTESIAN_POINT('Ctrl Pts',(178.537807503284,0.0149175389192058,
38.4283524243692));
#19511=CARTESIAN_POINT('Ctrl Pts',(178.540562605001,0.0145270880491169,
38.4206441795725));
#19512=CARTESIAN_POINT('Ctrl Pts',(178.548129056013,0.0124870215921244,
38.3998601077916));
#19513=CARTESIAN_POINT('Ctrl Pts',(178.587627771362,0.00738392785094328,
38.2924874843148));
#19514=CARTESIAN_POINT('Ctrl Pts',(178.614538362218,0.00313671619344931,
38.2181107712228));
#19515=CARTESIAN_POINT('Ctrl Pts',(178.647624171299,0.00102987596989992,
38.1266989348736));
#19516=CARTESIAN_POINT('Ctrl Pts',(178.666537253803,0.000407918176736971,
38.0738320437369));
#19517=CARTESIAN_POINT('Ctrl Pts',(178.669110050143,1.11050312057989E-15,
38.0664089817677));
#19518=CARTESIAN_POINT('Ctrl Pts',(178.670972086323,1.11022302462515E-15,
38.061269873677));
#19519=CARTESIAN_POINT('Ctrl Pts',(178.412949235465,0.0221748194567917,
38.3827594988839));
#19520=CARTESIAN_POINT('Ctrl Pts',(178.416788815217,0.0212514804521959,
38.3719446039049));
#19521=CARTESIAN_POINT('Ctrl Pts',(178.428787456164,0.018059442750159,38.3379328437124));
#19522=CARTESIAN_POINT('Ctrl Pts',(178.479303492309,0.00868912423993776,
38.1971252772954));
#19523=CARTESIAN_POINT('Ctrl Pts',(178.520861801226,0.0033049704669746,
38.0831735428938));
#19524=CARTESIAN_POINT('Ctrl Pts',(178.565879979014,0.000430856897763508,
37.9603421260445));
#19525=CARTESIAN_POINT('Ctrl Pts',(178.592381442498,-1.56457495638545E-5,
37.8878951389657));
#19526=CARTESIAN_POINT('Ctrl Pts',(178.597384099455,5.55111512312573E-16,
37.8741283338417));
#19527=CARTESIAN_POINT('Ctrl Pts',(178.6,5.55111512312573E-16,37.8669048105155));
#19528=CARTESIAN_POINT('',(178.787524038921,0.00040297784403398,38.5195382753398));
#19529=CARTESIAN_POINT('Ctrl Pts',(178.812916258969,1.77635683940025E-15,
38.45));
#19530=CARTESIAN_POINT('Ctrl Pts',(178.812792389797,1.77661612872642E-15,
38.4503392180603));
#19531=CARTESIAN_POINT('Ctrl Pts',(178.812666912028,2.29080308876542E-8,
38.4506828414828));
#19532=CARTESIAN_POINT('Ctrl Pts',(178.812507168468,1.04590663241311E-7,
38.451120307067));
#19533=CARTESIAN_POINT('Ctrl Pts',(178.812339990782,1.90074632413641E-7,
38.4515781313736));
#19534=CARTESIAN_POINT('Ctrl Pts',(178.812135423681,3.38991576868653E-7,
38.4521383523834));
#19535=CARTESIAN_POINT('Ctrl Pts',(178.811876024071,6.76277157829475E-7,
38.4528487410224));
#19536=CARTESIAN_POINT('Ctrl Pts',(178.811582600925,1.05780200312327E-6,
38.4536523061046));
#19537=CARTESIAN_POINT('Ctrl Pts',(178.81121902708,1.68218510003301E-6,
38.454647990168));
#19538=CARTESIAN_POINT('Ctrl Pts',(178.81078427153,2.84078831658263E-6,
38.4558386172768));
#19539=CARTESIAN_POINT('Ctrl Pts',(178.810308592603,4.10845041919785E-6,
38.4571413176687));
#19540=CARTESIAN_POINT('Ctrl Pts',(178.809748146625,6.030430202368E-6,38.4586761668976));
#19541=CARTESIAN_POINT('Ctrl Pts',(178.809125174397,8.98260863735345E-6,
38.4603822551952));
#19542=CARTESIAN_POINT('Ctrl Pts',(178.808193484876,1.33977552344303E-5,
38.4629338048754));
#19543=CARTESIAN_POINT('Ctrl Pts',(178.807123623568,2.02240544095713E-5,
38.4658637622743));
#19544=CARTESIAN_POINT('Ctrl Pts',(178.806029976226,2.96381288054093E-5,
38.4688588617692));
#19545=CARTESIAN_POINT('Ctrl Pts',(178.805292443249,3.59867843904441E-5,
38.4708786944512));
#19546=CARTESIAN_POINT('Ctrl Pts',(178.804545203554,4.34635709253636E-5,
38.4729251106001));
#19547=CARTESIAN_POINT('Ctrl Pts',(178.803814942525,5.17716369792254E-5,
38.474925026849));
#19548=CARTESIAN_POINT('Ctrl Pts',(178.80317860389,5.90111625757292E-5,
38.4766677242206));
#19549=CARTESIAN_POINT('Ctrl Pts',(178.802555399229,6.6863151583119E-5,
38.4783744513132));
#19550=CARTESIAN_POINT('Ctrl Pts',(178.801949204039,7.51735349577842E-5,
38.4800345928624));
#19551=CARTESIAN_POINT('Ctrl Pts',(178.801382229325,8.29462413561495E-5,
38.481587324218));
#19552=CARTESIAN_POINT('Ctrl Pts',(178.800830323152,9.11060767190131E-5,
38.483098785948));
#19553=CARTESIAN_POINT('Ctrl Pts',(178.800280785453,9.97858253111161E-5,
38.4846037562484));
#19554=CARTESIAN_POINT('Ctrl Pts',(178.799730342786,0.000108479867530143,
38.4861112049022));
#19555=CARTESIAN_POINT('Ctrl Pts',(178.799179179204,0.000117743550685572,
38.4876206225174));
#19556=CARTESIAN_POINT('Ctrl Pts',(178.798613206839,0.000127862606367657,
38.4891705875312));
#19557=CARTESIAN_POINT('Ctrl Pts',(178.798000470497,0.000138817758135477,
38.4908486197997));
#19558=CARTESIAN_POINT('Ctrl Pts',(178.797370559065,0.000150785769506228,
38.4925736784058));
#19559=CARTESIAN_POINT('Ctrl Pts',(178.79672645219,0.000163820813490645,
38.4943376017011));
#19560=CARTESIAN_POINT('Ctrl Pts',(178.795973597268,0.000179056634472028,
38.4963993377092));
#19561=CARTESIAN_POINT('Ctrl Pts',(178.795201645712,0.000195768932648973,
38.4985133566153));
#19562=CARTESIAN_POINT('Ctrl Pts',(178.794439465589,0.00021337220547224,
38.50060060215));
#19563=CARTESIAN_POINT('Ctrl Pts',(178.793524503989,0.000234504111399393,
38.5031062428186));
#19564=CARTESIAN_POINT('Ctrl Pts',(178.792625243217,0.0002569141979263,
38.5055688657824));
#19565=CARTESIAN_POINT('Ctrl Pts',(178.791809195932,0.000278444418397861,
38.5078035940878));
#19566=CARTESIAN_POINT('Ctrl Pts',(178.791180207023,0.000295039375735335,
38.509526066969));
#19567=CARTESIAN_POINT('Ctrl Pts',(178.790601441912,0.000311061767359691,
38.5111109936911));
#19568=CARTESIAN_POINT('Ctrl Pts',(178.79009691346,0.000325452799612158,
38.5124926209708));
#19569=CARTESIAN_POINT('Ctrl Pts',(178.789638615777,0.000338525157990883,
38.5137476474782));
#19570=CARTESIAN_POINT('Ctrl Pts',(178.789241892366,0.000350230035308143,
38.5148340510745));
#19571=CARTESIAN_POINT('Ctrl Pts',(178.788911958311,0.000360129645157414,
38.5157375543241));
#19572=CARTESIAN_POINT('Ctrl Pts',(178.78860236805,0.00036941884325196,
38.516585347398));
#19573=CARTESIAN_POINT('Ctrl Pts',(178.788351785867,0.000377107969535637,
38.5172715489645));
#19574=CARTESIAN_POINT('Ctrl Pts',(178.788149176854,0.000383380392984911,
38.5178263793466));
#19575=CARTESIAN_POINT('Ctrl Pts',(178.787959584021,0.000389249858125049,
38.5183455658481));
#19576=CARTESIAN_POINT('Ctrl Pts',(178.787812084152,0.000393876622551518,
38.5187494837048));
#19577=CARTESIAN_POINT('Ctrl Pts',(178.787681864855,0.000397984058347234,
38.5191060801148));
#19578=CARTESIAN_POINT('Ctrl Pts',(178.787627357716,0.000399703347116144,
38.519255344092));
#19579=CARTESIAN_POINT('Ctrl Pts',(178.787575672948,0.000401338993554701,
38.519396879218));
#19580=CARTESIAN_POINT('Ctrl Pts',(178.787524038921,0.000402977844033536,
38.5195382753398));
#19581=CARTESIAN_POINT('Ctrl Pts',(178.412949235465,0.0221748194567917,
38.3827594988839));
#19582=CARTESIAN_POINT('Ctrl Pts',(178.537807503284,0.0149175389192058,
38.4283524243692));
#19583=CARTESIAN_POINT('Ctrl Pts',(178.662665771103,0.00766025838161988,
38.4739453498545));
#19584=CARTESIAN_POINT('Ctrl Pts',(178.787524038921,0.00040297784403398,
38.5195382753398));
#19585=CARTESIAN_POINT('Ctrl Pts',(178.412949235465,0.0221748194567911,
38.3827594988839));
#19586=CARTESIAN_POINT('Ctrl Pts',(178.240471017511,0.0636522405289915,
38.8685766805066));
#19587=CARTESIAN_POINT('Ctrl Pts',(178.066773051231,0.169426085453293,39.3947605243754));
#19588=CARTESIAN_POINT('Ctrl Pts',(177.858376073723,0.4624110846645,40.2928391623376));
#19589=CARTESIAN_POINT('Ctrl Pts',(177.799999999912,0.62257825368506,40.6717586072261));
#19590=CARTESIAN_POINT('Ctrl Pts',(177.8,0.800000000395797,41.0213168380085));
#19591=CARTESIAN_POINT('Ctrl Pts',(178.537807503284,0.0149175389192054,
38.4283524243692));
#19592=CARTESIAN_POINT('Ctrl Pts',(178.363766365304,0.0444484291304303,
38.9141666714197));
#19593=CARTESIAN_POINT('Ctrl Pts',(178.18361402036,0.137778888719998,39.439427238818));
#19594=CARTESIAN_POINT('Ctrl Pts',(177.955395603962,0.414097686712283,40.3338925283666));
#19595=CARTESIAN_POINT('Ctrl Pts',(177.885823288757,0.568803257711311,40.7106223452905));
#19596=CARTESIAN_POINT('Ctrl Pts',(177.872973082299,0.743827073473452,41.0573334705988));
#19597=CARTESIAN_POINT('Ctrl Pts',(178.662665771103,0.00766025838161969,
38.4739453498545));
#19598=CARTESIAN_POINT('Ctrl Pts',(178.486833473156,0.0252372669559836,
38.9597325112783));
#19599=CARTESIAN_POINT('Ctrl Pts',(178.300397971406,0.106138282654787,39.4840892505963));
#19600=CARTESIAN_POINT('Ctrl Pts',(178.05241766608,0.365784202340891,40.374947182902));
#19601=CARTESIAN_POINT('Ctrl Pts',(177.971553852029,0.515058096066276,40.7494851784996));
#19602=CARTESIAN_POINT('Ctrl Pts',(177.945946164598,0.687654146551106,41.0933501031891));
#19603=CARTESIAN_POINT('Ctrl Pts',(178.787524038921,0.00040297784403398,
38.5195382753398));
#19604=CARTESIAN_POINT('Ctrl Pts',(178.61012882095,0.00603345555742248,
39.0053225021914));
#19605=CARTESIAN_POINT('Ctrl Pts',(178.417238940535,0.0744910859214918,
39.528755965039));
#19606=CARTESIAN_POINT('Ctrl Pts',(178.149437196319,0.317470804388674,40.416000548931));
#19607=CARTESIAN_POINT('Ctrl Pts',(178.057377140874,0.461283100092528,40.7883489165639));
#19608=CARTESIAN_POINT('Ctrl Pts',(178.018919246896,0.631481219628761,41.1293667357794));
#19609=CARTESIAN_POINT('',(178.018919246896,0.631481219628701,41.1293667357793));
#19610=CARTESIAN_POINT('Ctrl Pts',(178.787524038921,0.00040297784403398,
38.5195382753398));
#19611=CARTESIAN_POINT('Ctrl Pts',(178.61012882095,0.00603345555742248,
39.0053225021914));
#19612=CARTESIAN_POINT('Ctrl Pts',(178.417238940535,0.0744910859214918,
39.528755965039));
#19613=CARTESIAN_POINT('Ctrl Pts',(178.149437196319,0.317470804388674,40.416000548931));
#19614=CARTESIAN_POINT('Ctrl Pts',(178.057377140874,0.461283100092528,40.7883489165639));
#19615=CARTESIAN_POINT('Ctrl Pts',(178.018919246896,0.631481219628761,41.1293667357794));
#19616=CARTESIAN_POINT('',(178.018919246896,0.631481219628701,41.1293667357793));
#19617=CARTESIAN_POINT('Origin',(177.9,6.00000000000001,38.45));
#19618=CARTESIAN_POINT('',(177.8,0.973333333333333,41.3435483791052));
#19619=CARTESIAN_POINT('',(178.,0.800000000000003,41.4433259094192));
#19620=CARTESIAN_POINT('',(177.8,0.973333333333333,41.3435483791052));
#19621=CARTESIAN_POINT('',(178.,3.00667409058085,43.65));
#19622=CARTESIAN_POINT('Origin',(178.,6.00000000000001,38.45));
#19623=CARTESIAN_POINT('',(177.8,3.10645162089482,43.4766666666667));
#19624=CARTESIAN_POINT('',(178.,3.00667409058085,43.65));
#19625=CARTESIAN_POINT('Origin',(177.8,6.00000000000001,38.45));
#19626=CARTESIAN_POINT('Ctrl Pts',(177.8,0.800000000395732,41.0213168380084));
#19627=CARTESIAN_POINT('Ctrl Pts',(177.8,0.85616853425096,41.1319806866355));
#19628=CARTESIAN_POINT('Ctrl Pts',(177.8,0.913326151321778,41.2393040181827));
#19629=CARTESIAN_POINT('Ctrl Pts',(177.8,0.973333333333334,41.3435483791052));
#19630=CARTESIAN_POINT('Ctrl Pts',(177.872973082299,0.743827073473389,41.0573334705987));
#19631=CARTESIAN_POINT('Ctrl Pts',(177.868914723125,0.799233317184012,41.1670960723289));
#19632=CARTESIAN_POINT('Ctrl Pts',(177.866666666667,0.856146146238369,41.2736016445264));
#19633=CARTESIAN_POINT('Ctrl Pts',(177.866666666667,0.915555555555557,41.3768075558765));
#19634=CARTESIAN_POINT('Ctrl Pts',(177.945946164598,0.687654146551045,41.093350103189));
#19635=CARTESIAN_POINT('Ctrl Pts',(177.937829446251,0.742298100117064,41.2022114580222));
#19636=CARTESIAN_POINT('Ctrl Pts',(177.933333333333,0.79896614115496,41.3078992708702));
#19637=CARTESIAN_POINT('Ctrl Pts',(177.933333333333,0.857777777777779,41.4100667326478));
#19638=CARTESIAN_POINT('Ctrl Pts',(178.018919246896,0.631481219628701,41.1293667357793));
#19639=CARTESIAN_POINT('Ctrl Pts',(178.006744169376,0.685362883050116,41.2373268437155));
#19640=CARTESIAN_POINT('Ctrl Pts',(178.,0.74178613607155,41.3421968972139));
#19641=CARTESIAN_POINT('Ctrl Pts',(178.,0.800000000000002,41.4433259094191));
#19642=CARTESIAN_POINT('Ctrl Pts',(177.8,0.973333333333334,41.3435483791052));
#19643=CARTESIAN_POINT('Ctrl Pts',(177.8,0.913326151321778,41.2393040181827));
#19644=CARTESIAN_POINT('Ctrl Pts',(177.8,0.85616853425096,41.1319806866355));
#19645=CARTESIAN_POINT('Ctrl Pts',(177.8,0.800000000395732,41.0213168380084));
#19646=CARTESIAN_POINT('Ctrl Pts',(178.018919246896,0.631481219628701,41.1293667357793));
#19647=CARTESIAN_POINT('Ctrl Pts',(178.006744169376,0.685362883050116,41.2373268437155));
#19648=CARTESIAN_POINT('Ctrl Pts',(178.,0.74178613607155,41.3421968972139));
#19649=CARTESIAN_POINT('Ctrl Pts',(178.,0.800000000000002,41.4433259094191));
#19650=CARTESIAN_POINT('Ctrl Pts',(177.8,3.42868316060635,43.6499999989011));
#19651=CARTESIAN_POINT('Ctrl Pts',(177.799999999778,3.74718302197855,43.8116577622765));
#19652=CARTESIAN_POINT('Ctrl Pts',(177.852262520974,4.10069604234112,43.9610343215402));
#19653=CARTESIAN_POINT('Ctrl Pts',(178.027580341374,4.92462867457202,44.2486946146566));
#19654=CARTESIAN_POINT('Ctrl Pts',(178.227442457241,5.54472605716147,44.3832148024821));
#19655=CARTESIAN_POINT('Ctrl Pts',(178.412949792571,6.06724207026202,44.4278253145154));
#19656=CARTESIAN_POINT('Ctrl Pts',(177.872973082248,3.39266652802731,43.706172925833));
#19657=CARTESIAN_POINT('Ctrl Pts',(177.884801501945,3.70854266993171,43.8657195742618));
#19658=CARTESIAN_POINT('Ctrl Pts',(177.94736184287,4.0600303778348,44.0100109505439));
#19659=CARTESIAN_POINT('Ctrl Pts',(178.14244940435,4.88027329102046,44.2832673714004));
#19660=CARTESIAN_POINT('Ctrl Pts',(178.350875881265,5.49908229532861,44.4034058024122));
#19661=CARTESIAN_POINT('Ctrl Pts',(178.537808064946,6.02164914272028,44.4350825564341));
#19662=CARTESIAN_POINT('Ctrl Pts',(177.945946164496,3.35664989544827,43.7623458527649));
#19663=CARTESIAN_POINT('Ctrl Pts',(177.969158641282,3.66999188322933,43.9195329256993));
#19664=CARTESIAN_POINT('Ctrl Pts',(178.042561961955,4.0193437759176,44.0590539599822));
#19665=CARTESIAN_POINT('Ctrl Pts',(178.257082225015,4.83596655149052,44.317714473429));
#19666=CARTESIAN_POINT('Ctrl Pts',(178.473297911834,5.45363322129503,44.4233504482635));
#19667=CARTESIAN_POINT('Ctrl Pts',(178.662666337321,5.97605621517853,44.4423397983527));
#19668=CARTESIAN_POINT('Ctrl Pts',(178.018919246744,3.32063326286924,43.8185187796968));
#19669=CARTESIAN_POINT('Ctrl Pts',(178.053960143449,3.63135153118249,43.9735947376847));
#19670=CARTESIAN_POINT('Ctrl Pts',(178.137661283851,3.97867811141129,44.1080305889859));
#19671=CARTESIAN_POINT('Ctrl Pts',(178.37195128799,4.79161116793896,44.3522872301728));
#19672=CARTESIAN_POINT('Ctrl Pts',(178.596731335858,5.40798945946218,44.4435414481936));
#19673=CARTESIAN_POINT('Ctrl Pts',(178.787524609695,5.93046328763679,44.4495970402714));
#19674=CARTESIAN_POINT('',(177.8,3.42868316035968,43.649999999388));
#19675=CARTESIAN_POINT('Ctrl Pts',(178.412949792571,6.06724207026202,44.4278253145154));
#19676=CARTESIAN_POINT('Ctrl Pts',(178.227442457241,5.54472605716147,44.3832148024821));
#19677=CARTESIAN_POINT('Ctrl Pts',(178.027580341374,4.92462867457202,44.2486946146566));
#19678=CARTESIAN_POINT('Ctrl Pts',(177.852262520974,4.10069604234112,43.9610343215402));
#19679=CARTESIAN_POINT('Ctrl Pts',(177.799999999778,3.74718302197855,43.8116577622765));
#19680=CARTESIAN_POINT('Ctrl Pts',(177.8,3.42868316060635,43.6499999989011));
#19681=CARTESIAN_POINT('',(178.018919246744,3.32063326286958,43.818518779697));
#19682=CARTESIAN_POINT('',(177.8,3.42868316035968,43.649999999388));
#19683=CARTESIAN_POINT('Ctrl Pts',(178.018919246744,3.32063326286924,43.8185187796968));
#19684=CARTESIAN_POINT('Ctrl Pts',(178.053960143449,3.63135153118249,43.9735947376847));
#19685=CARTESIAN_POINT('Ctrl Pts',(178.137661283851,3.97867811141129,44.1080305889859));
#19686=CARTESIAN_POINT('Ctrl Pts',(178.37195128799,4.79161116793896,44.3522872301728));
#19687=CARTESIAN_POINT('Ctrl Pts',(178.596731335858,5.40798945946218,44.4435414481936));
#19688=CARTESIAN_POINT('Ctrl Pts',(178.787524609695,5.93046328763679,44.4495970402714));
#19689=CARTESIAN_POINT('Ctrl Pts',(177.8,3.10645162089482,43.4766666666667));
#19690=CARTESIAN_POINT('Ctrl Pts',(177.8,3.20794511515403,43.5350903408981));
#19691=CARTESIAN_POINT('Ctrl Pts',(177.8,3.31591505255455,43.5927634272858));
#19692=CARTESIAN_POINT('Ctrl Pts',(177.8,3.42868316060669,43.6499999989013));
#19693=CARTESIAN_POINT('Ctrl Pts',(177.866666666667,3.0731924441235,43.5344444444444));
#19694=CARTESIAN_POINT('Ctrl Pts',(177.866666666667,3.17367489207974,43.5922861203885));
#19695=CARTESIAN_POINT('Ctrl Pts',(177.86883755389,3.28081680397103,43.6497131392107));
#19696=CARTESIAN_POINT('Ctrl Pts',(177.872973082248,3.39266652802765,43.7061729258332));
#19697=CARTESIAN_POINT('Ctrl Pts',(177.933333333333,3.03993326735218,43.5922222222222));
#19698=CARTESIAN_POINT('Ctrl Pts',(177.933333333333,3.13940466900545,43.649481899879));
#19699=CARTESIAN_POINT('Ctrl Pts',(177.93767510778,3.24571855538751,43.7066628511355));
#19700=CARTESIAN_POINT('Ctrl Pts',(177.945946164496,3.35664989544862,43.7623458527651));
#19701=CARTESIAN_POINT('Ctrl Pts',(178.,3.00667409058085,43.65));
#19702=CARTESIAN_POINT('Ctrl Pts',(178.,3.10513444593116,43.7066776793694));
#19703=CARTESIAN_POINT('Ctrl Pts',(178.00651266167,3.21062030680399,43.7636125630604));
#19704=CARTESIAN_POINT('Ctrl Pts',(178.018919246744,3.32063326286958,43.818518779697));
#19705=CARTESIAN_POINT('Ctrl Pts',(177.8,3.42868316060669,43.6499999989013));
#19706=CARTESIAN_POINT('Ctrl Pts',(177.8,3.31591505255455,43.5927634272858));
#19707=CARTESIAN_POINT('Ctrl Pts',(177.8,3.20794511515403,43.5350903408981));
#19708=CARTESIAN_POINT('Ctrl Pts',(177.8,3.10645162089482,43.4766666666667));
#19709=CARTESIAN_POINT('Ctrl Pts',(178.,3.00667409058085,43.65));
#19710=CARTESIAN_POINT('Ctrl Pts',(178.,3.10513444593116,43.7066776793694));
#19711=CARTESIAN_POINT('Ctrl Pts',(178.00651266167,3.21062030680399,43.7636125630604));
#19712=CARTESIAN_POINT('Ctrl Pts',(178.018919246744,3.32063326286958,43.818518779697));
#19713=CARTESIAN_POINT('Origin',(177.8,63.5,-31.75));
#19714=CARTESIAN_POINT('',(177.8,123.993325909419,43.65));
#19715=CARTESIAN_POINT('',(177.8,92.25,43.65));
#19716=CARTESIAN_POINT('',(177.8,126.2,41.4433259094192));
#19717=CARTESIAN_POINT('Origin',(177.8,121.,38.45));
#19718=CARTESIAN_POINT('',(177.8,126.2,-104.943325909419));
#19719=CARTESIAN_POINT('',(177.8,126.2,-66.85));
#19720=CARTESIAN_POINT('',(177.8,123.993325909419,-107.15));
#19721=CARTESIAN_POINT('Origin',(177.8,121.,-101.95));
#19722=CARTESIAN_POINT('',(177.8,34.75,-107.15));
#19723=CARTESIAN_POINT('Ctrl Pts',(181.949550208499,0.0221746857420428,
38.3827579327069));
#19724=CARTESIAN_POINT('Ctrl Pts',(181.93931132845,0.0197124559678562,38.3539182157356));
#19725=CARTESIAN_POINT('Ctrl Pts',(181.84754199691,-0.000377263094500332,
38.0974645231953));
#19726=CARTESIAN_POINT('Ctrl Pts',(181.77034781043,2.07279408068869E-16,
37.8885753052303));
#19727=CARTESIAN_POINT('Ctrl Pts',(181.7625,5.55111512312556E-16,37.8669048105155));
#19728=CARTESIAN_POINT('Ctrl Pts',(181.824691935409,0.0149174437260072,
38.4283508582629));
#19729=CARTESIAN_POINT('Ctrl Pts',(181.817345007617,0.013876249080669,38.4077955695789));
#19730=CARTESIAN_POINT('Ctrl Pts',(181.752629283213,-0.00242179847811128,
38.2259457666522));
#19731=CARTESIAN_POINT('Ctrl Pts',(181.69711408673,8.79071517678641E-16,
38.076687125913));
#19732=CARTESIAN_POINT('Ctrl Pts',(181.691527913677,1.11022302462513E-15,
38.061269873677));
#19733=CARTESIAN_POINT('Ctrl Pts',(181.69983366232,0.00766020170997153,
38.4739437838189));
#19734=CARTESIAN_POINT('Ctrl Pts',(181.695441999281,0.00742672173854637,
38.4617486824133));
#19735=CARTESIAN_POINT('Ctrl Pts',(181.655779237654,0.00233129106079364,
38.3525367447957));
#19736=CARTESIAN_POINT('Ctrl Pts',(181.62388036303,1.55087664284178E-15,
38.2647989465957));
#19737=CARTESIAN_POINT('Ctrl Pts',(181.620555827354,1.66533453693771E-15,
38.2556349368385));
#19738=CARTESIAN_POINT('Ctrl Pts',(181.57497538923,0.000402959693935889,
38.5195367093749));
#19739=CARTESIAN_POINT('Ctrl Pts',(181.573558278095,0.000357981970936656,
38.5156560509973));
#19740=CARTESIAN_POINT('Ctrl Pts',(181.560928464961,-7.92708613026129E-6,
38.481069555198));
#19741=CARTESIAN_POINT('Ctrl Pts',(181.550646639331,2.22267096288126E-15,
38.4529107672783));
#19742=CARTESIAN_POINT('Ctrl Pts',(181.549583741031,2.22044604925029E-15,
38.45));
#19743=CARTESIAN_POINT('',(181.949550208499,0.0221746857420428,38.3827579327069));
#19744=CARTESIAN_POINT('Ctrl Pts',(181.7625,4.44089209850063E-16,37.8669048105155));
#19745=CARTESIAN_POINT('Ctrl Pts',(181.76304148203,4.20005004317793E-16,
37.8684000280116));
#19746=CARTESIAN_POINT('Ctrl Pts',(181.763584479695,5.09304599544949E-7,
37.8698993823924));
#19747=CARTESIAN_POINT('Ctrl Pts',(181.764185485109,1.77553950320153E-6,
37.8715567677798));
#19748=CARTESIAN_POINT('Ctrl Pts',(181.764814435413,3.10065040867961E-6,
37.8732912164553));
#19749=CARTESIAN_POINT('Ctrl Pts',(181.765506905312,5.25009810737027E-6,
37.8751987104973));
#19750=CARTESIAN_POINT('Ctrl Pts',(181.766307739637,9.06185204052612E-6,
37.8774013223017));
#19751=CARTESIAN_POINT('Ctrl Pts',(181.767138138677,1.30143259816557E-5,
37.879685248786));
#19752=CARTESIAN_POINT('Ctrl Pts',(181.768084982826,1.87485342410978E-5,
37.882286296731));
#19753=CARTESIAN_POINT('Ctrl Pts',(181.769177981748,2.78726356962578E-5,
37.8852852358398));
#19754=CARTESIAN_POINT('Ctrl Pts',(181.770320300149,3.74084447238513E-5,
37.8884194963221));
#19755=CARTESIAN_POINT('Ctrl Pts',(181.771622177173,5.06509191333375E-5,
37.8919881335616));
#19756=CARTESIAN_POINT('Ctrl Pts',(181.773096907529,7.01871096291384E-5,
37.896027172726));
#19757=CARTESIAN_POINT('Ctrl Pts',(181.774657138679,9.08559545094126E-5,
37.9003003842292));
#19758=CARTESIAN_POINT('Ctrl Pts',(181.776410738128,0.000118594684243597,
37.9050998197267));
#19759=CARTESIAN_POINT('Ctrl Pts',(181.778352315947,0.000157075370967652,
37.9104106590806));
#19760=CARTESIAN_POINT('Ctrl Pts',(181.780451023138,0.000198670249723156,
37.9161512977704));
#19761=CARTESIAN_POINT('Ctrl Pts',(181.782769206869,0.000252878342011502,
37.9224890235653));
#19762=CARTESIAN_POINT('Ctrl Pts',(181.785278039374,0.000324340171413695,
37.9293453635552));
#19763=CARTESIAN_POINT('Ctrl Pts',(181.788122975606,0.000405375612125061,
37.937120234943));
#19764=CARTESIAN_POINT('Ctrl Pts',(181.791212773971,0.000508738325902519,
37.9455611859274));
#19765=CARTESIAN_POINT('Ctrl Pts',(181.794481379312,0.000639510998152626,
37.9544887994803));
#19766=CARTESIAN_POINT('Ctrl Pts',(181.799555799721,0.000842531995694803,
37.9683486753855));
#19767=CARTESIAN_POINT('Ctrl Pts',(181.805059381922,0.00111289751450502,
37.9833765823867));
#19768=CARTESIAN_POINT('Ctrl Pts',(181.810697440792,0.00145319066376182,
37.998773281532));
#19769=CARTESIAN_POINT('Ctrl Pts',(181.814293586,0.00167024117814912,38.0085938185504));
#19770=CARTESIAN_POINT('Ctrl Pts',(181.817943390686,0.00191521782814626,
38.0185615609443));
#19771=CARTESIAN_POINT('Ctrl Pts',(181.821578859223,0.0021844270804634,
38.0284922998829));
#19772=CARTESIAN_POINT('Ctrl Pts',(181.824987110976,0.00243681075451073,
38.0378023676378));
#19773=CARTESIAN_POINT('Ctrl Pts',(181.828382262706,0.00271034782317473,
38.0470785394244));
#19774=CARTESIAN_POINT('Ctrl Pts',(181.831725566481,0.00300073968331871,
38.0562161880863));
#19775=CARTESIAN_POINT('Ctrl Pts',(181.834646587955,0.0032544530508039,
38.0641996887662));
#19776=CARTESIAN_POINT('Ctrl Pts',(181.837528033025,0.0035209403924873,
38.072077438301));
#19777=CARTESIAN_POINT('Ctrl Pts',(181.84036024516,0.00379790114339729,
38.0798239992515));
#19778=CARTESIAN_POINT('Ctrl Pts',(181.843021786712,0.00405817209476014,
38.0871037483919));
#19779=CARTESIAN_POINT('Ctrl Pts',(181.84563977042,0.00432762707091396,
38.0942674097725));
#19780=CARTESIAN_POINT('Ctrl Pts',(181.848222212492,0.00460594527901903,
38.1013379934289));
#19781=CARTESIAN_POINT('Ctrl Pts',(181.850701024556,0.00487309494308377,
38.1081248438525));
#19782=CARTESIAN_POINT('Ctrl Pts',(181.853147008996,0.00514835430903795,
38.1148256972557));
#19783=CARTESIAN_POINT('Ctrl Pts',(181.855583689387,0.00543381221564498,
38.1215063521776));
#19784=CARTESIAN_POINT('Ctrl Pts',(181.858071001312,0.00572520162318504,
38.1283258237515));
#19785=CARTESIAN_POINT('Ctrl Pts',(181.860551411675,0.00602752312911085,
38.1351319692169));
#19786=CARTESIAN_POINT('Ctrl Pts',(181.863055940733,0.00634484643309796,
38.1420115697532));
#19787=CARTESIAN_POINT('Ctrl Pts',(181.865640315095,0.0066722861202117,
38.1491104944738));
#19788=CARTESIAN_POINT('Ctrl Pts',(181.868250295974,0.00701574757250298,
38.1562874412164));
#19789=CARTESIAN_POINT('Ctrl Pts',(181.870899527483,0.00737805831443783,
38.1635813068402));
#19790=CARTESIAN_POINT('Ctrl Pts',(181.873695982834,0.00776050349121822,
38.1712805092238));
#19791=CARTESIAN_POINT('Ctrl Pts',(181.876536050774,0.00816400147160706,
38.1791096716376));
#19792=CARTESIAN_POINT('Ctrl Pts',(181.879415035157,0.00858931359615633,
38.1870569678962));
#19793=CARTESIAN_POINT('Ctrl Pts',(181.882513643039,0.00904707068189298,
38.1956105241314));
#19794=CARTESIAN_POINT('Ctrl Pts',(181.885657154427,0.00953016157912426,
38.2043004729611));
#19795=CARTESIAN_POINT('Ctrl Pts',(181.888818575754,0.0100356859835848,
38.2130529045922));
#19796=CARTESIAN_POINT('Ctrl Pts',(181.892379707013,0.0106051256667839,
38.2229119378085));
#19797=CARTESIAN_POINT('Ctrl Pts',(181.895963258973,0.0112031276223819,
38.2328494834971));
#19798=CARTESIAN_POINT('Ctrl Pts',(181.899508342925,0.0118193646321622,
38.2426964227595));
#19799=CARTESIAN_POINT('Ctrl Pts',(181.906183227132,0.0129796504642326,
38.2612367959178));
#19800=CARTESIAN_POINT('Ctrl Pts',(181.912718758197,0.0142069749798927,
38.2794495139526));
#19801=CARTESIAN_POINT('Ctrl Pts',(181.918632200457,0.0153837014308582,
38.2959720321497));
#19802=CARTESIAN_POINT('Ctrl Pts',(181.921657512848,0.0159857137540303,
38.3044249394131));
#19803=CARTESIAN_POINT('Ctrl Pts',(181.924519594541,0.0165735780399693,
38.3124338071031));
#19804=CARTESIAN_POINT('Ctrl Pts',(181.927164975675,0.0171299943247164,
38.3198448741925));
#19805=CARTESIAN_POINT('Ctrl Pts',(181.929548820379,0.0176314003402352,
38.3265232438267));
#19806=CARTESIAN_POINT('Ctrl Pts',(181.931756490456,0.0181071304378864,
38.3327155370088));
#19807=CARTESIAN_POINT('Ctrl Pts',(181.933762899352,0.0185468540560407,
38.3383480472888));
#19808=CARTESIAN_POINT('Ctrl Pts',(181.935639369544,0.0189581003699228,
38.3436157859203));
#19809=CARTESIAN_POINT('Ctrl Pts',(181.937339669048,0.0193377715846431,
38.3483934857085));
#19810=CARTESIAN_POINT('Ctrl Pts',(181.93885852085,0.0196810446211592,38.3526637724704));
#19811=CARTESIAN_POINT('Ctrl Pts',(181.940271287443,0.0200003415252573,
38.3566357982273));
#19812=CARTESIAN_POINT('Ctrl Pts',(181.941527033176,0.0202881189884772,
38.3601687015716));
#19813=CARTESIAN_POINT('Ctrl Pts',(181.942636217166,0.0205444571591845,
38.3632902746199));
#19814=CARTESIAN_POINT('Ctrl Pts',(181.943711761215,0.0207930209653079,
38.3663171748893));
#19815=CARTESIAN_POINT('Ctrl Pts',(181.94464940078,0.0210119940283042,38.3689570326758));
#19816=CARTESIAN_POINT('Ctrl Pts',(181.945474089021,0.021205750697401,38.3712791369017));
#19817=CARTESIAN_POINT('Ctrl Pts',(181.946277108126,0.0213944163034733,
38.3735402265622));
#19818=CARTESIAN_POINT('Ctrl Pts',(181.946972949247,0.021559156053933,38.3754998027936));
#19819=CARTESIAN_POINT('Ctrl Pts',(181.947600825471,0.0217084836580261,
38.3772679633097));
#19820=CARTESIAN_POINT('Ctrl Pts',(181.948209078132,0.0218531441962382,
38.3789808619627));
#19821=CARTESIAN_POINT('Ctrl Pts',(181.94875350008,0.0219833332935568,38.3805139890893));
#19822=CARTESIAN_POINT('Ctrl Pts',(181.949286053238,0.0221112095448139,
38.3820139178392));
#19823=CARTESIAN_POINT('Ctrl Pts',(181.949374298298,0.0221323988802871,
38.3822624588557));
#19824=CARTESIAN_POINT('Ctrl Pts',(181.949462255764,0.022153535006527,38.3825101974093));
#19825=CARTESIAN_POINT('Ctrl Pts',(181.949550208499,0.0221746857420413,
38.3827579327069));
#19826=CARTESIAN_POINT('',(181.57497538923,0.000402959693935889,38.5195367093749));
#19827=CARTESIAN_POINT('Ctrl Pts',(181.57497538923,0.000402959693935889,
38.5195367093749));
#19828=CARTESIAN_POINT('Ctrl Pts',(181.69983366232,0.00766020170997153,
38.4739437838189));
#19829=CARTESIAN_POINT('Ctrl Pts',(181.824691935409,0.0149174437260072,
38.4283508582629));
#19830=CARTESIAN_POINT('Ctrl Pts',(181.949550208499,0.0221746857420428,
38.3827579327069));
#19831=CARTESIAN_POINT('Ctrl Pts',(181.57497538923,0.000402959693936111,
38.5195367093749));
#19832=CARTESIAN_POINT('Ctrl Pts',(181.574851529658,0.00039902851210055,
38.519197528716));
#19833=CARTESIAN_POINT('Ctrl Pts',(181.574726061451,0.000395069178890136,
38.5188539427319));
#19834=CARTESIAN_POINT('Ctrl Pts',(181.574566326858,0.000390081041366841,
38.518416520908));
#19835=CARTESIAN_POINT('Ctrl Pts',(181.574399158571,0.000384860766966021,
38.5179587424408));
#19836=CARTESIAN_POINT('Ctrl Pts',(181.574194600227,0.000378517204501205,
38.5173985742044));
#19837=CARTESIAN_POINT('Ctrl Pts',(181.573935208538,0.000370621645222613,
38.5166882477071));
#19838=CARTESIAN_POINT('Ctrl Pts',(181.573641794121,0.000361690476534324,
38.5158847522804));
#19839=CARTESIAN_POINT('Ctrl Pts',(181.573278227823,0.000350775602826365,
38.5148891495373));
#19840=CARTESIAN_POINT('Ctrl Pts',(181.572843478859,0.000338135634860848,
38.5136986128781));
#19841=CARTESIAN_POINT('Ctrl Pts',(181.572367805852,0.000324305834040387,
38.5123960079261));
#19842=CARTESIAN_POINT('Ctrl Pts',(181.571807364196,0.000308439823463236,
38.5108612635613));
#19843=CARTESIAN_POINT('Ctrl Pts',(181.571184395662,0.000291619369626517,
38.5091552820435));
#19844=CARTESIAN_POINT('Ctrl Pts',(181.570252722647,0.000266463744452544,
38.5066039221317));
#19845=CARTESIAN_POINT('Ctrl Pts',(181.569182879842,0.000239333604321804,
38.503674166543));
#19846=CARTESIAN_POINT('Ctrl Pts',(181.568089252669,0.000214035990966366,
38.5006792470363));
#19847=CARTESIAN_POINT('Ctrl Pts',(181.567351730344,0.000196975739463386,
38.4986595276542));
#19848=CARTESIAN_POINT('Ctrl Pts',(181.566604501957,0.000180735411225578,
38.4966132148558));
#19849=CARTESIAN_POINT('Ctrl Pts',(181.565874252981,0.000165865156090739,
38.4946133876972));
#19850=CARTESIAN_POINT('Ctrl Pts',(181.565237923904,0.000152907416969221,
38.49287076537));
#19851=CARTESIAN_POINT('Ctrl Pts',(181.564614729409,0.00014097893488106,
38.4911641027617));
#19852=CARTESIAN_POINT('Ctrl Pts',(181.564008544896,0.000130048672500216,
38.4895040144456));
#19853=CARTESIAN_POINT('Ctrl Pts',(181.563441576379,0.00011982552339432,
38.487951322498));
#19854=CARTESIAN_POINT('Ctrl Pts',(181.562889677075,0.000110467742542563,
38.4864398910591));
#19855=CARTESIAN_POINT('Ctrl Pts',(181.562340146278,0.000101705034171395,
38.4849349404768));
#19856=CARTESIAN_POINT('Ctrl Pts',(181.561789713655,9.2927945483311E-5,
38.4834275201481));
#19857=CARTESIAN_POINT('Ctrl Pts',(181.561238560062,8.46975944274953E-5,
38.4819181200221));
#19858=CARTESIAN_POINT('Ctrl Pts',(181.56067259846,7.68526057823848E-5,
38.4803681636429));
#19859=CARTESIAN_POINT('Ctrl Pts',(181.560059870002,6.83593656547746E-5,
38.4786901304027));
#19860=CARTESIAN_POINT('Ctrl Pts',(181.559429967136,6.03338773008794E-5,
38.4769650596898));
#19861=CARTESIAN_POINT('Ctrl Pts',(181.558785869966,5.29249154554989E-5,
38.4752011147451));
#19862=CARTESIAN_POINT('Ctrl Pts',(181.558033019287,4.42649768435077E-5,
38.4731393339917));
#19863=CARTESIAN_POINT('Ctrl Pts',(181.557261073166,3.64754843892193E-5,
38.471025256065));
#19864=CARTESIAN_POINT('Ctrl Pts',(181.556498900774,2.98872215322987E-5,
38.4689379451134));
#19865=CARTESIAN_POINT('Ctrl Pts',(181.555583979329,2.19785869096659E-5,
38.4664323104691));
#19866=CARTESIAN_POINT('Ctrl Pts',(181.554684761097,1.58465131801333E-5,
38.4639696816724));
#19867=CARTESIAN_POINT('Ctrl Pts',(181.553868752768,1.14757415285993E-5,
38.4617349378622));
#19868=CARTESIAN_POINT('Ctrl Pts',(181.553239785674,8.10681568953756E-6,
38.4600124305416));
#19869=CARTESIAN_POINT('Ctrl Pts',(181.552661041472,5.75943763824285E-6,
38.4584274674403));
#19870=CARTESIAN_POINT('Ctrl Pts',(181.552156531242,4.1369507819411E-6,
38.4570458067133));
#19871=CARTESIAN_POINT('Ctrl Pts',(181.551698249181,2.66313206549139E-6,
38.4557907472771));
#19872=CARTESIAN_POINT('Ctrl Pts',(181.551301539411,1.77618418147096E-6,
38.4547043140198));
#19873=CARTESIAN_POINT('Ctrl Pts',(181.550971615919,1.20383124357915E-6,
38.4538007858999));
#19874=CARTESIAN_POINT('Ctrl Pts',(181.550662035304,6.66769231341577E-7,
38.4529529687611));
#19875=CARTESIAN_POINT('Ctrl Pts',(181.550411460152,4.02524086533268E-7,
38.4522667477014));
#19876=CARTESIAN_POINT('Ctrl Pts',(181.550208854898,2.44216733058522E-7,
38.4517118997389));
#19877=CARTESIAN_POINT('Ctrl Pts',(181.550019265284,9.60792622203152E-8,
38.4511926959744));
#19878=CARTESIAN_POINT('Ctrl Pts',(181.549871765901,4.12476565666961E-8,
38.4507887629029));
#19879=CARTESIAN_POINT('Ctrl Pts',(181.549741543983,1.55625716757868E-8,
38.4504321467835));
#19880=CARTESIAN_POINT('Ctrl Pts',(181.549687045568,4.81325671682278E-9,
38.4502829014529));
#19881=CARTESIAN_POINT('Ctrl Pts',(181.549635367948,1.77646490753008E-15,
38.4501413812976));
#19882=CARTESIAN_POINT('Ctrl Pts',(181.549583741031,1.77635683940025E-15,
38.45));
#19883=CARTESIAN_POINT('Ctrl Pts',(181.574975961468,5.93046172357687,44.4495970221434));
#19884=CARTESIAN_POINT('Ctrl Pts',(181.574444532932,5.93191700291845,44.4496138895458));
#19885=CARTESIAN_POINT('Ctrl Pts',(181.572770787455,5.93650035880571,44.449672474836));
#19886=CARTESIAN_POINT('Ctrl Pts',(181.565836964823,5.95548859185619,44.449843301418));
#19887=CARTESIAN_POINT('Ctrl Pts',(181.560226126263,5.97085451379058,44.4499402615516));
#19888=CARTESIAN_POINT('Ctrl Pts',(181.554178821344,5.98741591022133,44.449992182184));
#19889=CARTESIAN_POINT('Ctrl Pts',(181.55061386901,5.99717895300097,44.4500002913724));
#19890=CARTESIAN_POINT('Ctrl Pts',(181.549938048485,5.9990297223651,44.45));
#19891=CARTESIAN_POINT('Ctrl Pts',(181.549583741031,6.,44.45));
#19892=CARTESIAN_POINT('Ctrl Pts',(181.699834229027,5.97605464978202,44.4423397416411));
#19893=CARTESIAN_POINT('Ctrl Pts',(181.698187347511,5.9806278348658,44.4424272990258));
#19894=CARTESIAN_POINT('Ctrl Pts',(181.691731181696,5.99844959657613,44.4431086533954));
#19895=CARTESIAN_POINT('Ctrl Pts',(181.672687746495,6.05087537581987,44.4450308050866));
#19896=CARTESIAN_POINT('Ctrl Pts',(181.652734774536,6.10580896795632,44.447239748624));
#19897=CARTESIAN_POINT('Ctrl Pts',(181.635298667028,6.15378029848288,44.4488972633241));
#19898=CARTESIAN_POINT('Ctrl Pts',(181.624637758958,6.18311746495192,44.4497882438633));
#19899=CARTESIAN_POINT('Ctrl Pts',(181.62166399917,6.19131037030118,44.45));
#19900=CARTESIAN_POINT('Ctrl Pts',(181.620555827354,6.1943650631615,44.45));
#19901=CARTESIAN_POINT('Ctrl Pts',(181.824692496587,6.02164757598718,44.4350824611388));
#19902=CARTESIAN_POINT('Ctrl Pts',(181.821937394915,6.02935582072027,44.4354729132427));
#19903=CARTESIAN_POINT('Ctrl Pts',(181.814368169928,6.0501471994832,44.4375133635835));
#19904=CARTESIAN_POINT('Ctrl Pts',(181.774869846903,6.15751878131652,44.4426163977142));
#19905=CARTESIAN_POINT('Ctrl Pts',(181.747959001421,6.23189616960441,44.4468636541891));
#19906=CARTESIAN_POINT('Ctrl Pts',(181.714874888603,6.32330353191465,44.4489702868513));
#19907=CARTESIAN_POINT('Ctrl Pts',(181.69596209178,6.37616965773883,44.4495922345424));
#19908=CARTESIAN_POINT('Ctrl Pts',(181.693389949855,6.38359101823726,44.45));
#19909=CARTESIAN_POINT('Ctrl Pts',(181.691527913677,6.388730126323,44.45));
#19910=CARTESIAN_POINT('Ctrl Pts',(181.949550764146,6.06724050219233,44.4278251806365));
#19911=CARTESIAN_POINT('Ctrl Pts',(181.945711184342,6.07805539712614,44.4287485196519));
#19912=CARTESIAN_POINT('Ctrl Pts',(181.933709998201,6.11207446414045,44.4319413603754));
#19913=CARTESIAN_POINT('Ctrl Pts',(181.883194320107,6.25288098876544,44.4413115590186));
#19914=CARTESIAN_POINT('Ctrl Pts',(181.841635780004,6.36683339813076,44.4466958050519));
#19915=CARTESIAN_POINT('Ctrl Pts',(181.79661916996,6.4896603408434,44.4495694591275));
#19916=CARTESIAN_POINT('Ctrl Pts',(181.770117979333,6.56210656250854,44.4500159173546));
#19917=CARTESIAN_POINT('Ctrl Pts',(181.76511590054,6.57587166617334,44.45));
#19918=CARTESIAN_POINT('Ctrl Pts',(181.7625,6.5830951894845,44.45));
#19919=CARTESIAN_POINT('',(181.549583741031,6.,44.45));
#19920=CARTESIAN_POINT('',(181.574975961468,5.93046172357687,44.4495970221434));
#19921=CARTESIAN_POINT('Ctrl Pts',(181.549583741031,6.,44.45));
#19922=CARTESIAN_POINT('Ctrl Pts',(181.549707610205,5.99966078193585,44.45));
#19923=CARTESIAN_POINT('Ctrl Pts',(181.549833087975,5.99931715850951,44.449999977092));
#19924=CARTESIAN_POINT('Ctrl Pts',(181.549992831536,5.99887969292094,44.4499998954093));
#19925=CARTESIAN_POINT('Ctrl Pts',(181.550160009223,5.99842186860979,44.4499998099254));
#19926=CARTESIAN_POINT('Ctrl Pts',(181.550364576326,5.99786164759481,44.4499996610084));
#19927=CARTESIAN_POINT('Ctrl Pts',(181.550623975936,5.9971512589496,44.4499993237228));
#19928=CARTESIAN_POINT('Ctrl Pts',(181.550917399083,5.99634769386081,44.449998942198));
#19929=CARTESIAN_POINT('Ctrl Pts',(181.551280972928,5.99535200978955,44.4499983178149));
#19930=CARTESIAN_POINT('Ctrl Pts',(181.551715728478,5.99416138267107,44.4499971592116));
#19931=CARTESIAN_POINT('Ctrl Pts',(181.552191407404,5.9928586822711,44.4499958915495));
#19932=CARTESIAN_POINT('Ctrl Pts',(181.552751853379,5.9913238330328,44.4499939695697));
#19933=CARTESIAN_POINT('Ctrl Pts',(181.553374825605,5.9896177447235,44.4499910173912));
#19934=CARTESIAN_POINT('Ctrl Pts',(181.554306515129,5.98706619500538,44.4499866022445));
#19935=CARTESIAN_POINT('Ctrl Pts',(181.555376376442,5.98413623755719,44.4499797759452));
#19936=CARTESIAN_POINT('Ctrl Pts',(181.55647002379,5.98114113800806,44.4499703618705));
#19937=CARTESIAN_POINT('Ctrl Pts',(181.557207556768,5.97912130529461,44.4499640132147));
#19938=CARTESIAN_POINT('Ctrl Pts',(181.557954796465,5.97707488911245,44.449956536428));
#19939=CARTESIAN_POINT('Ctrl Pts',(181.558685057496,5.97507497283002,44.4499482283617));
#19940=CARTESIAN_POINT('Ctrl Pts',(181.559321396133,5.9733322754311,44.4499409888359));
#19941=CARTESIAN_POINT('Ctrl Pts',(181.559944600795,5.97162554831108,44.4499331368467));
#19942=CARTESIAN_POINT('Ctrl Pts',(181.560550795988,5.96996540673538,44.449924826463));
#19943=CARTESIAN_POINT('Ctrl Pts',(181.561117770701,5.96841267536218,44.4499170537564));
#19944=CARTESIAN_POINT('Ctrl Pts',(181.561669676874,5.96690121361503,44.4499088939209));
#19945=CARTESIAN_POINT('Ctrl Pts',(181.562219214574,5.96539624329965,44.4499002141721));
#19946=CARTESIAN_POINT('Ctrl Pts',(181.562769657243,5.96388879462565,44.4498915201296));
#19947=CARTESIAN_POINT('Ctrl Pts',(181.563320820828,5.96237937699256,44.4498822564462));
#19948=CARTESIAN_POINT('Ctrl Pts',(181.563886793199,5.96082941196163,44.4498721373903));
#19949=CARTESIAN_POINT('Ctrl Pts',(181.564499529544,5.95915137968164,44.4498611822383));
#19950=CARTESIAN_POINT('Ctrl Pts',(181.565129440981,5.95742632106529,44.4498492142267));
#19951=CARTESIAN_POINT('Ctrl Pts',(181.565773547862,5.95566239775938,44.4498361791825));
#19952=CARTESIAN_POINT('Ctrl Pts',(181.566526402788,5.95360066175229,44.4498209433614));
#19953=CARTESIAN_POINT('Ctrl Pts',(181.567298354351,5.9514866428474,44.449804231063));
#19954=CARTESIAN_POINT('Ctrl Pts',(181.568060534484,5.94939939730955,44.44978662779));
#19955=CARTESIAN_POINT('Ctrl Pts',(181.568975496117,5.9468937565782,44.4497654958833));
#19956=CARTESIAN_POINT('Ctrl Pts',(181.569874756927,5.94443113354704,44.4497430857959));
#19957=CARTESIAN_POINT('Ctrl Pts',(181.57069080425,5.94219640517704,44.4497215555745));
#19958=CARTESIAN_POINT('Ctrl Pts',(181.571319793182,5.94047393226165,44.4497049606166));
#19959=CARTESIAN_POINT('Ctrl Pts',(181.571898558316,5.93888900550459,44.4496889382245));
#19960=CARTESIAN_POINT('Ctrl Pts',(181.57240308679,5.9375073781912,44.4496745471917));
#19961=CARTESIAN_POINT('Ctrl Pts',(181.572861384492,5.93625235165496,44.4496614748328));
#19962=CARTESIAN_POINT('Ctrl Pts',(181.573258107921,5.93516594803045,44.449649769955));
#19963=CARTESIAN_POINT('Ctrl Pts',(181.573588041993,5.93426244475501,44.4496398703448));
#19964=CARTESIAN_POINT('Ctrl Pts',(181.573897632268,5.93341465165737,44.4496305811463));
#19965=CARTESIAN_POINT('Ctrl Pts',(181.574148214464,5.93272845006904,44.4496228920196));
#19966=CARTESIAN_POINT('Ctrl Pts',(181.574350823487,5.93217361966883,44.4496166195959));
#19967=CARTESIAN_POINT('Ctrl Pts',(181.574540416331,5.93165443315097,44.4496107501305));
#19968=CARTESIAN_POINT('Ctrl Pts',(181.574687916207,5.93125051528096,44.4496061233658));
#19969=CARTESIAN_POINT('Ctrl Pts',(181.574818135509,5.93089391886264,44.4496020159299));
#19970=CARTESIAN_POINT('Ctrl Pts',(181.574872642657,5.93074465486329,44.4496002966408));
#19971=CARTESIAN_POINT('Ctrl Pts',(181.574924327433,5.93060311971796,44.4495986609941));
#19972=CARTESIAN_POINT('Ctrl Pts',(181.574975961468,5.93046172357687,44.4495970221434));
#19973=CARTESIAN_POINT('',(181.949550764146,6.06724050219233,44.4278251806365));
#19974=CARTESIAN_POINT('Ctrl Pts',(181.949550764146,6.06724050219233,44.4278251806365));
#19975=CARTESIAN_POINT('Ctrl Pts',(181.824692496587,6.02164757598718,44.4350824611388));
#19976=CARTESIAN_POINT('Ctrl Pts',(181.699834229027,5.97605464978202,44.4423397416411));
#19977=CARTESIAN_POINT('Ctrl Pts',(181.574975961468,5.93046172357687,44.4495970221434));
#19978=CARTESIAN_POINT('',(181.7625,6.5830951894845,44.45));
#19979=CARTESIAN_POINT('Ctrl Pts',(181.949550764146,6.06724050219233,44.4278251806365));
#19980=CARTESIAN_POINT('Ctrl Pts',(181.94902079535,6.06873325846841,44.4279526270998));
#19981=CARTESIAN_POINT('Ctrl Pts',(181.948489242811,6.0702301556008,44.4280799229918));
#19982=CARTESIAN_POINT('Ctrl Pts',(181.947901535215,6.07188520706795,44.4282199372542));
#19983=CARTESIAN_POINT('Ctrl Pts',(181.94728649341,6.07361723477844,44.428366463563));
#19984=CARTESIAN_POINT('Ctrl Pts',(181.946609960367,6.07552244719632,44.4285269212254));
#19985=CARTESIAN_POINT('Ctrl Pts',(181.945828468642,6.07772300647724,44.4287109043704));
#19986=CARTESIAN_POINT('Ctrl Pts',(181.945018113731,6.08000484000598,44.4289016826478));
#19987=CARTESIAN_POINT('Ctrl Pts',(181.944094971134,6.08260405095877,44.4291177455792));
#19988=CARTESIAN_POINT('Ctrl Pts',(181.943030000191,6.08560145944807,44.4293644327469));
#19989=CARTESIAN_POINT('Ctrl Pts',(181.941916949163,6.08873419149441,44.4296222570636));
#19990=CARTESIAN_POINT('Ctrl Pts',(181.940649054564,6.09230165446145,44.4299135097798));
#19991=CARTESIAN_POINT('Ctrl Pts',(181.939212886804,6.09633987852072,44.4302387811672));
#19992=CARTESIAN_POINT('Ctrl Pts',(181.937693398372,6.10061238408365,44.4305829234911));
#19993=CARTESIAN_POINT('Ctrl Pts',(181.93598564529,6.10541155385979,44.4309650964571));
#19994=CARTESIAN_POINT('Ctrl Pts',(181.934093970544,6.11072251487221,44.4313805150329));
#19995=CARTESIAN_POINT('Ctrl Pts',(181.932049062151,6.11646368616331,44.4318295842683));
#19996=CARTESIAN_POINT('Ctrl Pts',(181.929789367954,6.12280248007158,44.4323174065243));
#19997=CARTESIAN_POINT('Ctrl Pts',(181.927341610279,6.12966028043394,44.4328328324238));
#19998=CARTESIAN_POINT('Ctrl Pts',(181.924565122129,6.13743907390991,44.4334174793095));
#19999=CARTESIAN_POINT('Ctrl Pts',(181.921546914366,6.1458848393179,44.4340374388843));
#20000=CARTESIAN_POINT('Ctrl Pts',(181.918349533181,6.15481772771552,44.4346724941065));
#20001=CARTESIAN_POINT('Ctrl Pts',(181.913396618503,6.16865525020576,44.4356562286534));
#20002=CARTESIAN_POINT('Ctrl Pts',(181.908015230853,6.18365673017568,44.4366745490118));
#20003=CARTESIAN_POINT('Ctrl Pts',(181.902486840944,6.19902659072339,44.4376570855153));
#20004=CARTESIAN_POINT('Ctrl Pts',(181.898955195236,6.2088451641123,44.4382847494253));
#20005=CARTESIAN_POINT('Ctrl Pts',(181.895364682588,6.21881124267631,44.4388980670532));
#20006=CARTESIAN_POINT('Ctrl Pts',(181.891781419326,6.22874060155642,44.4394848412838));
#20007=CARTESIAN_POINT('Ctrl Pts',(181.888422110018,6.23804937550653,44.440034942125));
#20008=CARTESIAN_POINT('Ctrl Pts',(181.885069687638,6.24732450257578,44.4405617369166));
#20009=CARTESIAN_POINT('Ctrl Pts',(181.881762187736,6.25646133484379,44.4410603836474));
#20010=CARTESIAN_POINT('Ctrl Pts',(181.878871956411,6.26444547985546,44.4414961219527));
#20011=CARTESIAN_POINT('Ctrl Pts',(181.876016047721,6.27232401048766,44.4419104549414));
#20012=CARTESIAN_POINT('Ctrl Pts',(181.873204044664,6.2800714641089,44.4423033601437));
#20013=CARTESIAN_POINT('Ctrl Pts',(181.870561055752,6.28735326060817,44.4426726499603));
#20014=CARTESIAN_POINT('Ctrl Pts',(181.867956945665,6.29451902766672,44.4430230545958));
#20015=CARTESIAN_POINT('Ctrl Pts',(181.865383784351,6.30159180112175,44.4433567463113));
#20016=CARTESIAN_POINT('Ctrl Pts',(181.862914409609,6.30837929945407,44.4436769788165));
#20017=CARTESIAN_POINT('Ctrl Pts',(181.860473628296,6.31508091628731,44.4439818551709));
#20018=CARTESIAN_POINT('Ctrl Pts',(181.858037986204,6.32176249133492,44.4442748222071));
#20019=CARTESIAN_POINT('Ctrl Pts',(181.855552642216,6.32858041110422,44.4445737675507));
#20020=CARTESIAN_POINT('Ctrl Pts',(181.85306986129,6.33538518338409,44.4448606695743));
#20021=CARTESIAN_POINT('Ctrl Pts',(181.85055859404,6.34226352247208,44.4451387828648));
#20022=CARTESIAN_POINT('Ctrl Pts',(181.847967136051,6.34936150329404,44.4454257769744));
#20023=CARTESIAN_POINT('Ctrl Pts',(181.845345405643,6.35653763295404,44.4457033474357));
#20024=CARTESIAN_POINT('Ctrl Pts',(181.84267965057,6.36383078704426,44.4459718736454));
#20025=CARTESIAN_POINT('Ctrl Pts',(181.839865757128,6.37152922816241,44.4462553220942));
#20026=CARTESIAN_POINT('Ctrl Pts',(181.837002917605,6.37935774694832,44.4465286150796));
#20027=CARTESIAN_POINT('Ctrl Pts',(181.834095833498,6.38730452968734,44.4467898321551));
#20028=CARTESIAN_POINT('Ctrl Pts',(181.830966994874,6.39585749886745,44.4470709750614));
#20029=CARTESIAN_POINT('Ctrl Pts',(181.827787062508,6.40454701082733,44.4473380241507));
#20030=CARTESIAN_POINT('Ctrl Pts',(181.824583454508,6.41329920717486,44.4475873899933));
#20031=CARTESIAN_POINT('Ctrl Pts',(181.820974942929,6.42315759242375,44.4478682731508));
#20032=CARTESIAN_POINT('Ctrl Pts',(181.817336668825,6.43309474070496,44.4481265525157));
#20033=CARTESIAN_POINT('Ctrl Pts',(181.8137310421,6.44294165689817,44.4483579274519));
#20034=CARTESIAN_POINT('Ctrl Pts',(181.806940176017,6.46148741725839,44.4487937008491));
#20035=CARTESIAN_POINT('Ctrl Pts',(181.800267516052,6.47970668562816,44.4491309639821));
#20036=CARTESIAN_POINT('Ctrl Pts',(181.794215639515,6.49623650830588,44.449371076666));
#20037=CARTESIAN_POINT('Ctrl Pts',(181.791120505867,6.50469041678578,44.4494938783859));
#20038=CARTESIAN_POINT('Ctrl Pts',(181.788188347131,6.51270076759385,44.4495920666799));
#20039=CARTESIAN_POINT('Ctrl Pts',(181.785475746618,6.52011386975146,44.4496700038562));
#20040=CARTESIAN_POINT('Ctrl Pts',(181.783031242769,6.5267943067218,44.4497402382038));
#20041=CARTESIAN_POINT('Ctrl Pts',(181.780765274131,6.53298908189307,44.4497941150971));
#20042=CARTESIAN_POINT('Ctrl Pts',(181.778704924533,6.53862447797697,44.449835858424));
#20043=CARTESIAN_POINT('Ctrl Pts',(181.77677798253,6.54389498228005,44.4498748988714));
#20044=CARTESIAN_POINT('Ctrl Pts',(181.775031043383,6.54867578880741,44.4499033746775));
#20045=CARTESIAN_POINT('Ctrl Pts',(181.773470463133,6.55294946200246,44.4499247770501));
#20046=CARTESIAN_POINT('Ctrl Pts',(181.772018885453,6.55692462997286,44.4499446845213));
#20047=CARTESIAN_POINT('Ctrl Pts',(181.770728582699,6.56046091928445,44.4499584916947));
#20048=CARTESIAN_POINT('Ctrl Pts',(181.769589326039,6.56358602529954,44.4499685877935));
#20049=CARTESIAN_POINT('Ctrl Pts',(181.768484615927,6.56661636634274,44.4499783777406));
#20050=CARTESIAN_POINT('Ctrl Pts',(181.767522032915,6.56925979952929,44.4499846840721));
#20051=CARTESIAN_POINT('Ctrl Pts',(181.766676133959,6.57158547767921,44.4499890998665));
#20052=CARTESIAN_POINT('Ctrl Pts',(181.765852458422,6.57385005571547,44.4499933996493));
#20053=CARTESIAN_POINT('Ctrl Pts',(181.765139502996,6.5758131168861,44.4499959037341));
#20054=CARTESIAN_POINT('Ctrl Pts',(181.764496879593,6.57758458469779,44.4499975077911));
#20055=CARTESIAN_POINT('Ctrl Pts',(181.763874348493,6.57930066568948,44.4499990616955));
#20056=CARTESIAN_POINT('Ctrl Pts',(181.763317868564,6.5808368131827,44.4499997670013));
#20057=CARTESIAN_POINT('Ctrl Pts',(181.762773707633,6.58233938708511,44.4499999531776));
#20058=CARTESIAN_POINT('Ctrl Pts',(181.762682266775,6.58259187975397,44.4499999844627));
#20059=CARTESIAN_POINT('Ctrl Pts',(181.762591132757,6.58284353633941,44.45));
#20060=CARTESIAN_POINT('Ctrl Pts',(181.7625,6.5830951894845,44.45));
#20061=CARTESIAN_POINT('',(181.656041870516,6.29154759474225,44.45));
#20062=CARTESIAN_POINT('Ctrl Pts',(181.949550764146,6.06724050219231,44.4278251806365));
#20063=CARTESIAN_POINT('Ctrl Pts',(182.122029380922,5.58142220595409,44.3863476637473));
#20064=CARTESIAN_POINT('Ctrl Pts',(182.295726981729,5.05523944602546,44.2805738182329));
#20065=CARTESIAN_POINT('Ctrl Pts',(182.504123999729,4.15716068129026,43.9875888528751));
#20066=CARTESIAN_POINT('Ctrl Pts',(182.562500000088,3.77824139277389,43.8274217463149));
#20067=CARTESIAN_POINT('Ctrl Pts',(182.5625,3.42868316199153,43.6499999996042));
#20068=CARTESIAN_POINT('Ctrl Pts',(181.824692496587,6.02164757598716,44.4350824611388));
#20069=CARTESIAN_POINT('Ctrl Pts',(181.998734032867,5.53583221576672,44.4055514751814));
#20070=CARTESIAN_POINT('Ctrl Pts',(182.178886012691,5.01057273132897,44.3122210149538));
#20071=CARTESIAN_POINT('Ctrl Pts',(182.407104469443,4.11610731539274,44.0359022508337));
#20072=CARTESIAN_POINT('Ctrl Pts',(182.476676711275,3.73937765462172,43.8811967422844));
#20073=CARTESIAN_POINT('Ctrl Pts',(182.489526917701,3.39266652940122,43.7061729265265));
#20074=CARTESIAN_POINT('Ctrl Pts',(181.699834229027,5.97605464978202,44.4423397416411));
#20075=CARTESIAN_POINT('Ctrl Pts',(181.875666121718,5.49026860678201,44.424762745888));
#20076=CARTESIAN_POINT('Ctrl Pts',(182.062102046114,4.96591082303663,44.3438616250727));
#20077=CARTESIAN_POINT('Ctrl Pts',(182.310082295719,4.07505300028109,44.0842157500705));
#20078=CARTESIAN_POINT('Ctrl Pts',(182.390946147939,3.70051482158828,43.934941903938));
#20079=CARTESIAN_POINT('Ctrl Pts',(182.416553835402,3.3566498968109,43.7623458534489));
#20080=CARTESIAN_POINT('Ctrl Pts',(181.574975961468,5.93046172357687,44.4495970221434));
#20081=CARTESIAN_POINT('Ctrl Pts',(181.752370773663,5.44467861659464,44.4439665573221));
#20082=CARTESIAN_POINT('Ctrl Pts',(181.945261077076,4.92124410834014,44.3755088217936));
#20083=CARTESIAN_POINT('Ctrl Pts',(182.213062765432,4.03399963438357,44.1325291480292));
#20084=CARTESIAN_POINT('Ctrl Pts',(182.305122859126,3.66165108343612,43.9887168999075));
#20085=CARTESIAN_POINT('Ctrl Pts',(182.343580753104,3.32063326422058,43.8185187803712));
#20086=CARTESIAN_POINT('',(182.343580753104,3.3206332642207,43.8185187803713));
#20087=CARTESIAN_POINT('Ctrl Pts',(181.574975961468,5.93046172357687,44.4495970221434));
#20088=CARTESIAN_POINT('Ctrl Pts',(181.752370773663,5.44467861659464,44.4439665573221));
#20089=CARTESIAN_POINT('Ctrl Pts',(181.945261077076,4.92124410834014,44.3755088217936));
#20090=CARTESIAN_POINT('Ctrl Pts',(182.213062765432,4.03399963438357,44.1325291480292));
#20091=CARTESIAN_POINT('Ctrl Pts',(182.305122859126,3.66165108343612,43.9887168999075));
#20092=CARTESIAN_POINT('Ctrl Pts',(182.343580753104,3.32063326422058,43.8185187803712));
#20093=CARTESIAN_POINT('',(182.5625,3.42868316190269,43.6499999997796));
#20094=CARTESIAN_POINT('',(182.343580753104,3.3206332642207,43.8185187803713));
#20095=CARTESIAN_POINT('Ctrl Pts',(182.5625,3.42868316199153,43.6499999996042));
#20096=CARTESIAN_POINT('Ctrl Pts',(182.562500000088,3.77824139277389,43.8274217463149));
#20097=CARTESIAN_POINT('Ctrl Pts',(182.504123999729,4.15716068129026,43.9875888528751));
#20098=CARTESIAN_POINT('Ctrl Pts',(182.295726981729,5.05523944602546,44.2805738182329));
#20099=CARTESIAN_POINT('Ctrl Pts',(182.122029380922,5.58142220595409,44.3863476637473));
#20100=CARTESIAN_POINT('Ctrl Pts',(181.949550764146,6.06724050219231,44.4278251806365));
#20101=CARTESIAN_POINT('Origin',(182.4625,6.00000000000001,38.45));
#20102=CARTESIAN_POINT('',(182.3625,0.800000000000003,41.4433259094192));
#20103=CARTESIAN_POINT('',(182.5625,0.973333333333333,41.3435483791052));
#20104=CARTESIAN_POINT('',(182.3625,0.800000000000003,41.4433259094192));
#20105=CARTESIAN_POINT('',(182.5625,3.10645162089482,43.4766666666667));
#20106=CARTESIAN_POINT('Origin',(182.5625,6.00000000000001,38.45));
#20107=CARTESIAN_POINT('',(182.3625,3.00667409058085,43.65));
#20108=CARTESIAN_POINT('',(182.5625,3.10645162089482,43.4766666666667));
#20109=CARTESIAN_POINT('Origin',(182.3625,6.00000000000001,38.45));
#20110=CARTESIAN_POINT('Ctrl Pts',(182.5625,3.42868316199165,43.6499999996043));
#20111=CARTESIAN_POINT('Ctrl Pts',(182.5625,3.31801931336449,43.593831465749));
#20112=CARTESIAN_POINT('Ctrl Pts',(182.5625,3.21069598181731,43.5366738486782));
#20113=CARTESIAN_POINT('Ctrl Pts',(182.5625,3.10645162089483,43.4766666666667));
#20114=CARTESIAN_POINT('Ctrl Pts',(182.489526917701,3.39266652940134,43.7061729265266));
#20115=CARTESIAN_POINT('Ctrl Pts',(182.493585276875,3.28290392767115,43.650766682816));
#20116=CARTESIAN_POINT('Ctrl Pts',(182.495833333333,3.17639835547358,43.5938538537616));
#20117=CARTESIAN_POINT('Ctrl Pts',(182.495833333333,3.07319244412351,43.5344444444445));
#20118=CARTESIAN_POINT('Ctrl Pts',(182.416553835402,3.35664989681102,43.762345853449));
#20119=CARTESIAN_POINT('Ctrl Pts',(182.424670553749,3.24778854197781,43.7077018998829));
#20120=CARTESIAN_POINT('Ctrl Pts',(182.429166666667,3.14210072912985,43.6510338588451));
#20121=CARTESIAN_POINT('Ctrl Pts',(182.429166666667,3.03993326735218,43.5922222222222));
#20122=CARTESIAN_POINT('Ctrl Pts',(182.343580753104,3.32063326422071,43.8185187803713));
#20123=CARTESIAN_POINT('Ctrl Pts',(182.355755830624,3.21267315628446,43.7646371169499));
#20124=CARTESIAN_POINT('Ctrl Pts',(182.3625,3.10780310278612,43.7082138639285));
#20125=CARTESIAN_POINT('Ctrl Pts',(182.3625,3.00667409058086,43.65));
#20126=CARTESIAN_POINT('Ctrl Pts',(182.5625,3.10645162089483,43.4766666666667));
#20127=CARTESIAN_POINT('Ctrl Pts',(182.5625,3.21069598181731,43.5366738486782));
#20128=CARTESIAN_POINT('Ctrl Pts',(182.5625,3.31801931336449,43.593831465749));
#20129=CARTESIAN_POINT('Ctrl Pts',(182.5625,3.42868316199165,43.6499999996043));
#20130=CARTESIAN_POINT('Ctrl Pts',(182.343580753104,3.32063326422071,43.8185187803713));
#20131=CARTESIAN_POINT('Ctrl Pts',(182.355755830624,3.21267315628446,43.7646371169499));
#20132=CARTESIAN_POINT('Ctrl Pts',(182.3625,3.10780310278612,43.7082138639285));
#20133=CARTESIAN_POINT('Ctrl Pts',(182.3625,3.00667409058086,43.65));
#20134=CARTESIAN_POINT('Ctrl Pts',(182.5625,0.800000001098831,41.0213168393936));
#20135=CARTESIAN_POINT('Ctrl Pts',(182.562500000222,0.638342237723523,40.7028169780214));
#20136=CARTESIAN_POINT('Ctrl Pts',(182.510237346477,0.488965591972109,40.349303524625));
#20137=CARTESIAN_POINT('Ctrl Pts',(182.334919667211,0.201305187631971,39.5253711428458));
#20138=CARTESIAN_POINT('Ctrl Pts',(182.135056358579,0.0667849130182742,
38.9052706332517));
#20139=CARTESIAN_POINT('Ctrl Pts',(181.949550208499,0.0221746857420428,
38.3827579327069));
#20140=CARTESIAN_POINT('Ctrl Pts',(182.489526917752,0.743827074166946,41.0573334719727));
#20141=CARTESIAN_POINT('Ctrl Pts',(182.477698497965,0.584280425725848,40.7414573298172));
#20142=CARTESIAN_POINT('Ctrl Pts',(182.415138024714,0.439988962986447,40.3899691894989));
#20143=CARTESIAN_POINT('Ctrl Pts',(182.220050603944,0.166732430848469,39.5697265255869));
#20144=CARTESIAN_POINT('Ctrl Pts',(182.011622935248,0.0465939131825897,
38.9509143970108));
#20145=CARTESIAN_POINT('Ctrl Pts',(181.824691935409,0.0149174437260072,
38.4283508582629));
#20146=CARTESIAN_POINT('Ctrl Pts',(182.416553835504,0.68765414723506,41.0933501045517));
#20147=CARTESIAN_POINT('Ctrl Pts',(182.393341358808,0.53046707431298,40.7800081170217));
#20148=CARTESIAN_POINT('Ctrl Pts',(182.319938208693,0.390945991654019,40.4306566666258));
#20149=CARTESIAN_POINT('Ctrl Pts',(182.105417882415,0.132285334982405,39.6140336660972));
#20150=CARTESIAN_POINT('Ctrl Pts',(181.889203292348,0.0266495899212865,
38.9963701019499));
#20151=CARTESIAN_POINT('Ctrl Pts',(181.69983366232,0.00766020170997153,
38.4739437838189));
#20152=CARTESIAN_POINT('Ctrl Pts',(182.343580753256,0.631481220303175,41.1293667371307));
#20153=CARTESIAN_POINT('Ctrl Pts',(182.308539856551,0.476405262315305,40.8186484688175));
#20154=CARTESIAN_POINT('Ctrl Pts',(182.22483888693,0.341969362668358,40.4713223314997));
#20155=CARTESIAN_POINT('Ctrl Pts',(181.990548819148,0.0977125781989031,
39.6583890488383));
#20156=CARTESIAN_POINT('Ctrl Pts',(181.765769869017,0.00645859008560202,
39.042013865709));
#20157=CARTESIAN_POINT('Ctrl Pts',(181.57497538923,0.000402959693935889,
38.5195367093749));
#20158=CARTESIAN_POINT('',(182.5625,0.800000000612018,41.0213168396403));
#20159=CARTESIAN_POINT('Ctrl Pts',(181.949550208499,0.0221746857420428,
38.3827579327069));
#20160=CARTESIAN_POINT('Ctrl Pts',(182.135056358579,0.0667849130182742,
38.9052706332517));
#20161=CARTESIAN_POINT('Ctrl Pts',(182.334919667211,0.201305187631971,39.5253711428458));
#20162=CARTESIAN_POINT('Ctrl Pts',(182.510237346477,0.488965591972109,40.349303524625));
#20163=CARTESIAN_POINT('Ctrl Pts',(182.562500000222,0.638342237723523,40.7028169780214));
#20164=CARTESIAN_POINT('Ctrl Pts',(182.5625,0.800000001098831,41.0213168393936));
#20165=CARTESIAN_POINT('',(182.343580753256,0.631481220303007,41.1293667371304));
#20166=CARTESIAN_POINT('',(182.5625,0.800000000612018,41.0213168396403));
#20167=CARTESIAN_POINT('Ctrl Pts',(182.343580753256,0.631481220303175,41.1293667371307));
#20168=CARTESIAN_POINT('Ctrl Pts',(182.308539856551,0.476405262315305,40.8186484688175));
#20169=CARTESIAN_POINT('Ctrl Pts',(182.22483888693,0.341969362668358,40.4713223314997));
#20170=CARTESIAN_POINT('Ctrl Pts',(181.990548819148,0.0977125781989031,
39.6583890488383));
#20171=CARTESIAN_POINT('Ctrl Pts',(181.765769869017,0.00645859008560202,
39.042013865709));
#20172=CARTESIAN_POINT('Ctrl Pts',(181.57497538923,0.000402959693935889,
38.5195367093749));
#20173=CARTESIAN_POINT('Ctrl Pts',(182.5625,0.973333333333336,41.3435483791052));
#20174=CARTESIAN_POINT('Ctrl Pts',(182.5625,0.914909659101875,41.242054884846));
#20175=CARTESIAN_POINT('Ctrl Pts',(182.5625,0.857236572714185,41.1340849474454));
#20176=CARTESIAN_POINT('Ctrl Pts',(182.5625,0.800000001098665,41.0213168393933));
#20177=CARTESIAN_POINT('Ctrl Pts',(182.495833333333,0.915555555555558,41.3768075558765));
#20178=CARTESIAN_POINT('Ctrl Pts',(182.495833333333,0.857713879611461,41.2763251079203));
#20179=CARTESIAN_POINT('Ctrl Pts',(182.49366244611,0.800286860789319,41.169183196029));
#20180=CARTESIAN_POINT('Ctrl Pts',(182.489526917752,0.743827074166782,41.0573334719723));
#20181=CARTESIAN_POINT('Ctrl Pts',(182.429166666667,0.857777777777781,41.4100667326478));
#20182=CARTESIAN_POINT('Ctrl Pts',(182.429166666667,0.800518100121046,41.3105953309945));
#20183=CARTESIAN_POINT('Ctrl Pts',(182.42482489222,0.743337148864453,41.2042814446125));
#20184=CARTESIAN_POINT('Ctrl Pts',(182.416553835504,0.687654147234898,41.0933501045513));
#20185=CARTESIAN_POINT('Ctrl Pts',(182.3625,0.800000000000004,41.4433259094192));
#20186=CARTESIAN_POINT('Ctrl Pts',(182.3625,0.743322320630632,41.3448655540688));
#20187=CARTESIAN_POINT('Ctrl Pts',(182.355987338329,0.686387436939587,41.239379693196));
#20188=CARTESIAN_POINT('Ctrl Pts',(182.343580753256,0.631481220303014,41.1293667371304));
#20189=CARTESIAN_POINT('Ctrl Pts',(182.5625,0.800000001098665,41.0213168393933));
#20190=CARTESIAN_POINT('Ctrl Pts',(182.5625,0.857236572714185,41.1340849474454));
#20191=CARTESIAN_POINT('Ctrl Pts',(182.5625,0.914909659101875,41.242054884846));
#20192=CARTESIAN_POINT('Ctrl Pts',(182.5625,0.973333333333336,41.3435483791052));
#20193=CARTESIAN_POINT('Ctrl Pts',(182.3625,0.800000000000004,41.4433259094192));
#20194=CARTESIAN_POINT('Ctrl Pts',(182.3625,0.743322320630632,41.3448655540688));
#20195=CARTESIAN_POINT('Ctrl Pts',(182.355987338329,0.686387436939587,41.239379693196));
#20196=CARTESIAN_POINT('Ctrl Pts',(182.343580753256,0.631481220303014,41.1293667371304));
#20197=CARTESIAN_POINT('Origin',(181.7625,0.800000000000001,3.35000000000001));
#20198=CARTESIAN_POINT('',(181.949550200389,0.0221746837918946,-101.88275790988));
#20199=CARTESIAN_POINT('Ctrl Pts',(181.949550200389,0.0221746837918912,
-101.88275790988));
#20200=CARTESIAN_POINT('Ctrl Pts',(181.949020231057,0.0220472376058877,
-101.881265152351));
#20201=CARTESIAN_POINT('Ctrl Pts',(181.948488677977,0.0219199419923545,
-101.879768253967));
#20202=CARTESIAN_POINT('Ctrl Pts',(181.947900969848,0.0217799280541142,
-101.878113201481));
#20203=CARTESIAN_POINT('Ctrl Pts',(181.947285927459,0.0216334020783753,
-101.876381172632));
#20204=CARTESIAN_POINT('Ctrl Pts',(181.946609393835,0.0214729447980497,
-101.874475959315));
#20205=CARTESIAN_POINT('Ctrl Pts',(181.945827901584,0.0212889621299003,
-101.872275399603));
#20206=CARTESIAN_POINT('Ctrl Pts',(181.945017546083,0.0210981843364628,
-101.869993565502));
#20207=CARTESIAN_POINT('Ctrl Pts',(181.944094402945,0.0208821219884184,
-101.867394354444));
#20208=CARTESIAN_POINT('Ctrl Pts',(181.943029431607,0.0206354355477969,
-101.864396946535));
#20209=CARTESIAN_POINT('Ctrl Pts',(181.941916380075,0.0203776119700361,
-101.861264214841));
#20210=CARTESIAN_POINT('Ctrl Pts',(181.940648485108,0.0200863601446586,
-101.857696752903));
#20211=CARTESIAN_POINT('Ctrl Pts',(181.939212317266,0.0197610898408669,
-101.853658530765));
#20212=CARTESIAN_POINT('Ctrl Pts',(181.937692828547,0.0194169486180327,
-101.849386026672));
#20213=CARTESIAN_POINT('Ctrl Pts',(181.93598507545,0.0190347769592833,-101.844586859225));
#20214=CARTESIAN_POINT('Ctrl Pts',(181.934093401175,0.0186193599318965,
-101.839275901635));
#20215=CARTESIAN_POINT('Ctrl Pts',(181.93204849278,0.0181702922577936,-101.833534732605));
#20216=CARTESIAN_POINT('Ctrl Pts',(181.929788799043,0.0176824718261296,
-101.827195941937));
#20217=CARTESIAN_POINT('Ctrl Pts',(181.927341042605,0.0171670480409611,
-101.82033814611));
#20218=CARTESIAN_POINT('Ctrl Pts',(181.924564553008,0.0165824029531123,
-101.812559349791));
#20219=CARTESIAN_POINT('Ctrl Pts',(181.921546344304,0.0159624454782107,
-101.804113581838));
#20220=CARTESIAN_POINT('Ctrl Pts',(181.91834896333,0.0153273927115106,-101.795180692153));
#20221=CARTESIAN_POINT('Ctrl Pts',(181.913396100735,0.0143436722478956,
-101.781343312265));
#20222=CARTESIAN_POINT('Ctrl Pts',(181.908014776974,0.0133253675338641,
-101.766342002379));
#20223=CARTESIAN_POINT('Ctrl Pts',(181.902486455809,0.0123428460364121,
-101.750972317255));
#20224=CARTESIAN_POINT('Ctrl Pts',(181.89895482528,0.0117151866054473,-101.741153776038));
#20225=CARTESIAN_POINT('Ctrl Pts',(181.895364328797,0.0111018734427425,
-101.731187729355));
#20226=CARTESIAN_POINT('Ctrl Pts',(181.891781082577,0.0105151035721518,
-101.721258401538));
#20227=CARTESIAN_POINT('Ctrl Pts',(181.888421789245,0.009965006818473,-101.71194965671));
#20228=CARTESIAN_POINT('Ctrl Pts',(181.885069383611,0.00943821602199506,
-101.70267455804));
#20229=CARTESIAN_POINT('Ctrl Pts',(181.881761901085,0.00893957313635096,
-101.69353775326));
#20230=CARTESIAN_POINT('Ctrl Pts',(181.878871682462,0.00850383781729341,
-101.685553625418));
#20231=CARTESIAN_POINT('Ctrl Pts',(181.876015787016,0.00808950773794182,
-101.677675111449));
#20232=CARTESIAN_POINT('Ctrl Pts',(181.873203797631,0.00769660533975813,
-101.669927674095));
#20233=CARTESIAN_POINT('Ctrl Pts',(181.870560822923,0.00732731834799652,
-101.662645896615));
#20234=CARTESIAN_POINT('Ctrl Pts',(181.867956727377,0.00697691642498478,
-101.655480148105));
#20235=CARTESIAN_POINT('Ctrl Pts',(181.865383580778,0.00664322728912792,
-101.64840739288));
#20236=CARTESIAN_POINT('Ctrl Pts',(181.862914219001,0.00632299710939984,
-101.641619908862));
#20237=CARTESIAN_POINT('Ctrl Pts',(181.86047345084,0.00601812297287069,
-101.634918306135));
#20238=CARTESIAN_POINT('Ctrl Pts',(181.858037821854,0.00572515802433116,
-101.628236745118));
#20239=CARTESIAN_POINT('Ctrl Pts',(181.855552491816,0.0054262148804763,
-101.621418841249));
#20240=CARTESIAN_POINT('Ctrl Pts',(181.853069724786,0.00513931491516174,
-101.614614084804));
#20241=CARTESIAN_POINT('Ctrl Pts',(181.850558471049,0.00486120351446528,
-101.60773576152));
#20242=CARTESIAN_POINT('Ctrl Pts',(181.847967027646,0.00457421142590764,
-101.60063779876));
#20243=CARTESIAN_POINT('Ctrl Pts',(181.845345311431,0.00429664280136511,
-101.593461687163));
#20244=CARTESIAN_POINT('Ctrl Pts',(181.842679569903,0.0040281182289359,
-101.586168551203));
#20245=CARTESIAN_POINT('Ctrl Pts',(181.839865690715,0.00374467150392575,
-101.578470129103));
#20246=CARTESIAN_POINT('Ctrl Pts',(181.83700286472,0.00347138002015111,
-101.570641629404));
#20247=CARTESIAN_POINT('Ctrl Pts',(181.834095793202,0.0032101642241178,
-101.56269486586));
#20248=CARTESIAN_POINT('Ctrl Pts',(181.830966968037,0.00292902268659486,
-101.554141917091));
#20249=CARTESIAN_POINT('Ctrl Pts',(181.827787048038,0.00266197470938195,
-101.545452425659));
#20250=CARTESIAN_POINT('Ctrl Pts',(181.824583451151,0.00241260974534963,
-101.536700249963));
#20251=CARTESIAN_POINT('Ctrl Pts',(181.820974951551,0.00213172753559789,
-101.526841886502));
#20252=CARTESIAN_POINT('Ctrl Pts',(181.817336687823,0.00187344882906896,
-101.516904760142));
#20253=CARTESIAN_POINT('Ctrl Pts',(181.813731069805,0.00164207432593222,
-101.507057866022));
#20254=CARTESIAN_POINT('Ctrl Pts',(181.806940226809,0.00120630217362233,
-101.488512165496));
#20255=CARTESIAN_POINT('Ctrl Pts',(181.800267583721,0.000869039289859969,
-101.470292956922));
#20256=CARTESIAN_POINT('Ctrl Pts',(181.794215716949,0.000628926406277541,
-101.453763189425));
#20257=CARTESIAN_POINT('Ctrl Pts',(181.791120585805,0.000506124485427283,
-101.445309302364));
#20258=CARTESIAN_POINT('Ctrl Pts',(181.788188427994,0.000407935916206988,
-101.437298972468));
#20259=CARTESIAN_POINT('Ctrl Pts',(181.785475826965,0.000329998452306857,
-101.429885890493));
#20260=CARTESIAN_POINT('Ctrl Pts',(181.783031322716,0.000259763847384077,
-101.423205471888));
#20261=CARTESIAN_POINT('Ctrl Pts',(181.780765352501,0.000205886685921585,
-101.417010714464));
#20262=CARTESIAN_POINT('Ctrl Pts',(181.778705000268,0.000164143110408577,
-101.411375335315));
#20263=CARTESIAN_POINT('Ctrl Pts',(181.776778055821,0.000125102430976801,
-101.406104846907));
#20264=CARTESIAN_POINT('Ctrl Pts',(181.775031113303,9.66264096144005E-5,
-101.401324055554));
#20265=CARTESIAN_POINT('Ctrl Pts',(181.773470528856,7.52238512622405E-5,
-101.397050396643));
#20266=CARTESIAN_POINT('Ctrl Pts',(181.772018947239,5.53162068281227E-5,
-101.393075241868));
#20267=CARTESIAN_POINT('Ctrl Pts',(181.770728639844,4.15088856209883E-5,
-101.389538965001));
#20268=CARTESIAN_POINT('Ctrl Pts',(181.769589377915,3.1412666232411E-5,
-101.386413870535));
#20269=CARTESIAN_POINT('Ctrl Pts',(181.768484662701,2.16226022730055E-5,
-101.383383540712));
#20270=CARTESIAN_POINT('Ctrl Pts',(181.767522073996,1.53161792071218E-5,
-101.380740117898));
#20271=CARTESIAN_POINT('Ctrl Pts',(181.766676168814,1.09003154893372E-5,
-101.378414449133));
#20272=CARTESIAN_POINT('Ctrl Pts',(181.765852487221,6.60046517202568E-6,
-101.376149880247));
#20273=CARTESIAN_POINT('Ctrl Pts',(181.765139525231,4.09633361300762E-6,
-101.374186827287));
#20274=CARTESIAN_POINT('Ctrl Pts',(181.764496894799,2.49224690684891E-6,
-101.372415366613));
#20275=CARTESIAN_POINT('Ctrl Pts',(181.763874356865,9.38313611751158E-7,
-101.370699292469));
#20276=CARTESIAN_POINT('Ctrl Pts',(181.76331786967,2.32994581050169E-7,
-101.369163150831));
#20277=CARTESIAN_POINT('Ctrl Pts',(181.762773701049,4.68201671877111E-8,
-101.36766058165));
#20278=CARTESIAN_POINT('Ctrl Pts',(181.76268226241,1.55366010411297E-8,
-101.367408099467));
#20279=CARTESIAN_POINT('Ctrl Pts',(181.762591130575,6.66121167867262E-16,
-101.367156453271));
#20280=CARTESIAN_POINT('Ctrl Pts',(181.7625,6.66133814775094E-16,-101.366904810515));
#20281=CARTESIAN_POINT('',(182.5625,0.800000000612023,-104.52131683964));
#20282=CARTESIAN_POINT('Ctrl Pts',(182.5625,0.800000001098851,-104.521316839394));
#20283=CARTESIAN_POINT('Ctrl Pts',(182.562500000222,0.638342237723529,-104.202816978021));
#20284=CARTESIAN_POINT('Ctrl Pts',(182.51023714977,0.488966122920897,-103.849303636982));
#20285=CARTESIAN_POINT('Ctrl Pts',(182.334918859392,0.201307103612158,-103.02537106626));
#20286=CARTESIAN_POINT('Ctrl Pts',(182.135056739364,0.0667850025429474,
-102.405271696106));
#20287=CARTESIAN_POINT('Ctrl Pts',(181.949550200389,0.022174683791894,-101.88275790988));
#20288=CARTESIAN_POINT('',(182.5625,0.800000000000001,3.35000000000001));
#20289=CARTESIAN_POINT('Origin',(177.8,6.00000000000001,38.45));
#20290=CARTESIAN_POINT('',(177.8,6.,44.45));
#20291=CARTESIAN_POINT('Ctrl Pts',(181.949550265183,6.06724190764558,-107.927825300627));
#20292=CARTESIAN_POINT('Ctrl Pts',(181.9393114125,6.09608154848852,-107.930287524609));
#20293=CARTESIAN_POINT('Ctrl Pts',(181.847546692115,6.35252593990272,-107.950381345263));
#20294=CARTESIAN_POINT('Ctrl Pts',(181.770347680097,6.56142467898131,-107.95));
#20295=CARTESIAN_POINT('Ctrl Pts',(181.7625,6.58309518948447,-107.95));
#20296=CARTESIAN_POINT('Ctrl Pts',(181.824691992404,6.02164898271766,-107.935082546577));
#20297=CARTESIAN_POINT('Ctrl Pts',(181.817345081843,6.04220422326554,-107.936123736651));
#20298=CARTESIAN_POINT('Ctrl Pts',(181.752634028788,6.22404472257607,-107.952425867466));
#20299=CARTESIAN_POINT('Ctrl Pts',(181.697114000682,6.37331286135213,-107.95));
#20300=CARTESIAN_POINT('Ctrl Pts',(181.691527913677,6.38873012632298,-107.95));
#20301=CARTESIAN_POINT('Ctrl Pts',(181.699833719625,5.97605605778975,-107.942339792527));
#20302=CARTESIAN_POINT('Ctrl Pts',(181.695442063896,5.98825113903972,-107.94257327241));
#20303=CARTESIAN_POINT('Ctrl Pts',(181.655779679084,6.09746188028193,-107.947668893388));
#20304=CARTESIAN_POINT('Ctrl Pts',(181.623880321266,6.18520104372295,-107.95));
#20305=CARTESIAN_POINT('Ctrl Pts',(181.620555827354,6.19436506316149,-107.95));
#20306=CARTESIAN_POINT('Ctrl Pts',(181.574975446846,5.93046313286183,-107.949597038478));
#20307=CARTESIAN_POINT('Ctrl Pts',(181.573558332847,5.93434379914083,-107.949642016394));
#20308=CARTESIAN_POINT('Ctrl Pts',(181.56092895885,5.9689290898352,-107.950008001077));
#20309=CARTESIAN_POINT('Ctrl Pts',(181.55064664185,5.99708922609377,-107.95));
#20310=CARTESIAN_POINT('Ctrl Pts',(181.549583741031,6.,-107.95));
#20311=CARTESIAN_POINT('',(181.7625,6.58309518948447,-107.95));
#20312=CARTESIAN_POINT('',(181.949550265183,6.06724190764558,-107.927825300627));
#20313=CARTESIAN_POINT('Ctrl Pts',(181.7625,6.58309518948447,-107.95));
#20314=CARTESIAN_POINT('Ctrl Pts',(181.763041473032,6.58159997091306,-107.95));
#20315=CARTESIAN_POINT('Ctrl Pts',(181.763584461698,6.58010061545635,-107.949999490713));
#20316=CARTESIAN_POINT('Ctrl Pts',(181.764185458177,6.57844322897763,-107.949998224517));
#20317=CARTESIAN_POINT('Ctrl Pts',(181.764814399128,6.5767087791675,-107.949996899447));
#20318=CARTESIAN_POINT('Ctrl Pts',(181.765506859744,6.57480128397547,-107.949994750064));
#20319=CARTESIAN_POINT('Ctrl Pts',(181.76630768495,6.57259867099715,-107.949990938408));
#20320=CARTESIAN_POINT('Ctrl Pts',(181.76713807453,6.57031474330569,-107.949986986036));
#20321=CARTESIAN_POINT('Ctrl Pts',(181.768084909396,6.5677136941309,-107.949981251966));
#20322=CARTESIAN_POINT('Ctrl Pts',(181.769177899328,6.56471475376686,-107.949972128052));
#20323=CARTESIAN_POINT('Ctrl Pts',(181.770320208327,6.56158049199346,-107.949962592439));
#20324=CARTESIAN_POINT('Ctrl Pts',(181.771622076268,6.55801185344115,-107.949949350216));
#20325=CARTESIAN_POINT('Ctrl Pts',(181.773096798008,6.55397281294379,-107.949929814341));
#20326=CARTESIAN_POINT('Ctrl Pts',(181.774657020027,6.5496996000754,-107.949909145831));
#20327=CARTESIAN_POINT('Ctrl Pts',(181.776410610864,6.54490016320143,-107.94988140751));
#20328=CARTESIAN_POINT('Ctrl Pts',(181.778352180765,6.53958932246262,-107.949842927308));
#20329=CARTESIAN_POINT('Ctrl Pts',(181.780450879358,6.53384868238663,-107.949801332955));
#20330=CARTESIAN_POINT('Ctrl Pts',(181.782769055297,6.527510955219,-107.949747125478));
#20331=CARTESIAN_POINT('Ctrl Pts',(181.785277881027,6.5206546138659,-107.949675664339));
#20332=CARTESIAN_POINT('Ctrl Pts',(181.788122809382,6.51287974146625,-107.949594629686));
#20333=CARTESIAN_POINT('Ctrl Pts',(181.791212601148,6.50443878957439,-107.94949126786));
#20334=CARTESIAN_POINT('Ctrl Pts',(181.794481201446,6.49551117516263,-107.949360496118));
#20335=CARTESIAN_POINT('Ctrl Pts',(181.799555618821,6.48165128482589,-107.949157476373));
#20336=CARTESIAN_POINT('Ctrl Pts',(181.805059202589,6.46662336130415,-107.948887112081));
#20337=CARTESIAN_POINT('Ctrl Pts',(181.810697267405,6.45122664552554,-107.948546819801));
#20338=CARTESIAN_POINT('Ctrl Pts',(181.814293413217,6.44140610660598,-107.948329770034));
#20339=CARTESIAN_POINT('Ctrl Pts',(181.817943220182,6.43143836252728,-107.948084794035));
#20340=CARTESIAN_POINT('Ctrl Pts',(181.821578692671,6.42150762201582,-107.947815585253));
#20341=CARTESIAN_POINT('Ctrl Pts',(181.824986948131,6.41219755278633,-107.94756320202));
#20342=CARTESIAN_POINT('Ctrl Pts',(181.82838210504,6.40292137962293,-107.947289665233));
#20343=CARTESIAN_POINT('Ctrl Pts',(181.831725415348,6.3937837295531,-107.946999273444));
#20344=CARTESIAN_POINT('Ctrl Pts',(181.834646442654,6.38580022730003,-107.946745560128));
#20345=CARTESIAN_POINT('Ctrl Pts',(181.837527894586,6.37792247617696,-107.946479072676));
#20346=CARTESIAN_POINT('Ctrl Pts',(181.840360114445,6.37017591351464,-107.946202111639));
#20347=CARTESIAN_POINT('Ctrl Pts',(181.843021663982,6.36289616078084,-107.945941840348));
#20348=CARTESIAN_POINT('Ctrl Pts',(181.845639656412,6.35573249576307,-107.945672384872));
#20349=CARTESIAN_POINT('Ctrl Pts',(181.848222107743,6.34866190828394,-107.94539406601));
#20350=CARTESIAN_POINT('Ctrl Pts',(181.850700927839,6.34187505653352,-107.945126915811));
#20351=CARTESIAN_POINT('Ctrl Pts',(181.853146920829,6.33517420157077,-107.944851655773));
#20352=CARTESIAN_POINT('Ctrl Pts',(181.855583610037,6.32849354473312,-107.94456619708));
#20353=CARTESIAN_POINT('Ctrl Pts',(181.858070930426,6.32167407267557,-107.944274806933));
#20354=CARTESIAN_POINT('Ctrl Pts',(181.860551349524,6.31486792632985,-107.943972484574));
#20355=CARTESIAN_POINT('Ctrl Pts',(181.863055887233,6.30798832458689,-107.943655160345));
#20356=CARTESIAN_POINT('Ctrl Pts',(181.865640271041,6.30088939719322,-107.943327719638));
#20357=CARTESIAN_POINT('Ctrl Pts',(181.868250261284,6.29371244740061,-107.942984257084));
#20358=CARTESIAN_POINT('Ctrl Pts',(181.870899501794,6.28641857841591,-107.942621945199));
#20359=CARTESIAN_POINT('Ctrl Pts',(181.873695966718,6.27871937228751,-107.942239498805));
#20360=CARTESIAN_POINT('Ctrl Pts',(181.876536043829,6.27089020577594,-107.94183599956));
#20361=CARTESIAN_POINT('Ctrl Pts',(181.87941503676,6.26294290518415,-107.941410686167));
#20362=CARTESIAN_POINT('Ctrl Pts',(181.882513653988,6.25438934388254,-107.940952927694));
#20363=CARTESIAN_POINT('Ctrl Pts',(181.885657174003,6.24569938970116,-107.940469835403));
#20364=CARTESIAN_POINT('Ctrl Pts',(181.888818603077,6.2369469526327,-107.939964309647));
#20365=CARTESIAN_POINT('Ctrl Pts',(181.892379743607,6.22708791178712,-107.939394868355));
#20366=CARTESIAN_POINT('Ctrl Pts',(181.895963303727,6.21715035833682,-107.938796864838));
#20367=CARTESIAN_POINT('Ctrl Pts',(181.89950839463,6.20730341159208,-107.93818062638));
#20368=CARTESIAN_POINT('Ctrl Pts',(181.906183290512,6.18876302826307,-107.937020338067));
#20369=CARTESIAN_POINT('Ctrl Pts',(181.912718828949,6.17055030095437,-107.935793011526));
#20370=CARTESIAN_POINT('Ctrl Pts',(181.918632275053,6.15402777629446,-107.934616283725));
#20371=CARTESIAN_POINT('Ctrl Pts',(181.921657588146,6.14557486925797,-107.934014270963));
#20372=CARTESIAN_POINT('Ctrl Pts',(181.924519669777,6.13756600214987,-107.933426406399));
#20373=CARTESIAN_POINT('Ctrl Pts',(181.927165050345,6.13015493599256,-107.93286998997));
#20374=CARTESIAN_POINT('Ctrl Pts',(181.929548894861,6.12347656629904,-107.932368583756));
#20375=CARTESIAN_POINT('Ctrl Pts',(181.931756564295,6.11728427347274,-107.931892853576));
#20376=CARTESIAN_POINT('Ctrl Pts',(181.933762972264,6.11165176399886,-107.931453129964));
#20377=CARTESIAN_POINT('Ctrl Pts',(181.935639441692,6.10638402583803,-107.931041883635));
#20378=CARTESIAN_POINT('Ctrl Pts',(181.937339740164,6.10160632696724,-107.930662212485));
#20379=CARTESIAN_POINT('Ctrl Pts',(181.938858590785,6.09733604159958,-107.930318939573));
#20380=CARTESIAN_POINT('Ctrl Pts',(181.940271356321,6.09336401702112,-107.929999642775));
#20381=CARTESIAN_POINT('Ctrl Pts',(181.941527100859,6.08983111529414,-107.929711865469));
#20382=CARTESIAN_POINT('Ctrl Pts',(181.942636283578,6.0867095443179,-107.929455527493));
#20383=CARTESIAN_POINT('Ctrl Pts',(181.943711826412,6.08368264601373,-107.929206963871));
#20384=CARTESIAN_POINT('Ctrl Pts',(181.944649464688,6.08104279063139,-107.928987991027));
#20385=CARTESIAN_POINT('Ctrl Pts',(181.945474151593,6.07872068925136,-107.928794234602));
#20386=CARTESIAN_POINT('Ctrl Pts',(181.946277169405,6.07645960233774,-107.928605569231));
#20387=CARTESIAN_POINT('Ctrl Pts',(181.946973009188,6.07450002927844,-107.92844082974));
#20388=CARTESIAN_POINT('Ctrl Pts',(181.947600884013,6.07273187234834,-107.928291502419));
#20389=CARTESIAN_POINT('Ctrl Pts',(181.948209135317,6.07101897717428,-107.928146842155));
#20390=CARTESIAN_POINT('Ctrl Pts',(181.948753555853,6.06948585391396,-107.928016653354));
#20391=CARTESIAN_POINT('Ctrl Pts',(181.949286107487,6.06798592939739,-107.927888777429));
#20392=CARTESIAN_POINT('Ctrl Pts',(181.949374353366,6.06773738606642,-107.92786758789));
#20393=CARTESIAN_POINT('Ctrl Pts',(181.94946231164,6.06748964522795,-107.927846451563));
#20394=CARTESIAN_POINT('Ctrl Pts',(181.949550265183,6.06724190764557,-107.927825300627));
#20395=CARTESIAN_POINT('Ctrl Pts',(181.574975446846,5.93046313286183,-107.949597038478));
#20396=CARTESIAN_POINT('Ctrl Pts',(181.699833719625,5.97605605778975,-107.942339792527));
#20397=CARTESIAN_POINT('Ctrl Pts',(181.824691992404,6.02164898271766,-107.935082546577));
#20398=CARTESIAN_POINT('Ctrl Pts',(181.949550265183,6.06724190764558,-107.927825300627));
#20399=CARTESIAN_POINT('',(181.656041870516,6.29154759474223,-107.95));
#20400=CARTESIAN_POINT('Ctrl Pts',(181.5749753816,0.000402959451920593,
-102.019536688494));
#20401=CARTESIAN_POINT('Ctrl Pts',(181.574443965076,0.000386092815958592,
-102.018081442042));
#20402=CARTESIAN_POINT('Ctrl Pts',(181.57276933122,0.000327472074650577,
-102.01349565333));
#20403=CARTESIAN_POINT('Ctrl Pts',(181.565835797325,0.000156658918309325,
-101.994508210116));
#20404=CARTESIAN_POINT('Ctrl Pts',(181.560224999407,5.96987181011011E-5,
-101.97914239978));
#20405=CARTESIAN_POINT('Ctrl Pts',(181.554178400524,7.80232307688747E-6,
-101.962582937518));
#20406=CARTESIAN_POINT('Ctrl Pts',(181.550613625885,-3.04359490813502E-7,
-101.952820381474));
#20407=CARTESIAN_POINT('Ctrl Pts',(181.549938040358,7.48801562377757E-30,
-101.950970255468));
#20408=CARTESIAN_POINT('Ctrl Pts',(181.549583741031,7.48801562377757E-30,
-101.95));
#20409=CARTESIAN_POINT('Ctrl Pts',(181.69983365453,0.00766020089857859,
-101.973943762289));
#20410=CARTESIAN_POINT('Ctrl Pts',(181.698186781027,0.00757264579072308,
-101.969370599695));
#20411=CARTESIAN_POINT('Ctrl Pts',(181.691729730125,0.00689126727407931,
-101.95154639469));
#20412=CARTESIAN_POINT('Ctrl Pts',(181.672686601652,0.00496913839755225,
-101.899121401405));
#20413=CARTESIAN_POINT('Ctrl Pts',(181.652733689967,0.00276020645176135,
-101.844187926299));
#20414=CARTESIAN_POINT('Ctrl Pts',(181.635298291474,0.00110271920042685,
-101.79621853881));
#20415=CARTESIAN_POINT('Ctrl Pts',(181.624637545854,0.000211744708212053,
-101.766881865813));
#20416=CARTESIAN_POINT('Ctrl Pts',(181.621664005803,1.85037170770867E-16,
-101.758689606456));
#20417=CARTESIAN_POINT('Ctrl Pts',(181.620555827354,1.85037170770867E-16,
-101.755634936838));
#20418=CARTESIAN_POINT('Ctrl Pts',(181.82469192746,0.0149174423452366,-101.928350836085));
#20419=CARTESIAN_POINT('Ctrl Pts',(181.821936829738,0.0145269932961417,
-101.920642603346));
#20420=CARTESIAN_POINT('Ctrl Pts',(181.814360476815,0.012485571334149,-101.89983249948));
#20421=CARTESIAN_POINT('Ctrl Pts',(181.7748633369,0.00738273680960432,-101.792464040696));
#20422=CARTESIAN_POINT('Ctrl Pts',(181.74795211748,0.00313538503982533,
-101.718085227754));
#20423=CARTESIAN_POINT('Ctrl Pts',(181.714872511107,0.00102928842360235,
-101.62668976236));
#20424=CARTESIAN_POINT('Ctrl Pts',(181.695960435895,0.000407368516516136,
-101.573825817795));
#20425=CARTESIAN_POINT('Ctrl Pts',(181.693389971248,3.70074341541726E-16,
-101.566408957444));
#20426=CARTESIAN_POINT('Ctrl Pts',(181.691527913677,3.70074341541726E-16,
-101.561269873677));
#20427=CARTESIAN_POINT('Ctrl Pts',(181.949550200389,0.0221746837918946,
-101.88275790988));
#20428=CARTESIAN_POINT('Ctrl Pts',(181.945710620478,0.0212513476946085,
-101.871943016518));
#20429=CARTESIAN_POINT('Ctrl Pts',(181.933702897428,0.0180564544770989,
-101.837905214242));
#20430=CARTESIAN_POINT('Ctrl Pts',(181.883188323836,0.00868662858135192,
-101.69710180877));
#20431=CARTESIAN_POINT('Ctrl Pts',(181.841629490353,0.00330219114123234,
-101.583147980247));
#20432=CARTESIAN_POINT('Ctrl Pts',(181.796617064414,0.000429725518060977,
-101.460332943123));
#20433=CARTESIAN_POINT('Ctrl Pts',(181.770116550723,-1.66216652364724E-5,
-101.387888909435));
#20434=CARTESIAN_POINT('Ctrl Pts',(181.765115936694,5.55111512312586E-16,
-101.374128308432));
#20435=CARTESIAN_POINT('Ctrl Pts',(181.7625,5.55111512312586E-16,-101.366904810515));
#20436=CARTESIAN_POINT('Ctrl Pts',(181.949550200389,0.0221746837918946,
-101.88275790988));
#20437=CARTESIAN_POINT('Ctrl Pts',(181.82469192746,0.0149174423452366,-101.928350836085));
#20438=CARTESIAN_POINT('Ctrl Pts',(181.69983365453,0.00766020089857859,
-101.973943762289));
#20439=CARTESIAN_POINT('Ctrl Pts',(181.5749753816,0.000402959451920593,
-102.019536688494));
#20440=CARTESIAN_POINT('Ctrl Pts',(181.949550200389,0.022174683791894,-101.88275790988));
#20441=CARTESIAN_POINT('Ctrl Pts',(182.135056739364,0.0667850025429474,
-102.405271696106));
#20442=CARTESIAN_POINT('Ctrl Pts',(182.334918859392,0.201307103612158,-103.02537106626));
#20443=CARTESIAN_POINT('Ctrl Pts',(182.51023714977,0.488966122920897,-103.849303636982));
#20444=CARTESIAN_POINT('Ctrl Pts',(182.562500000222,0.638342237723529,-104.202816978021));
#20445=CARTESIAN_POINT('Ctrl Pts',(182.5625,0.800000001098851,-104.521316839394));
#20446=CARTESIAN_POINT('Ctrl Pts',(181.82469192746,0.0149174423452362,-101.928350836085));
#20447=CARTESIAN_POINT('Ctrl Pts',(182.011623315591,0.0465940030836249,
-102.450915459268));
#20448=CARTESIAN_POINT('Ctrl Pts',(182.220049796037,0.16673434696279,-103.0697264493));
#20449=CARTESIAN_POINT('Ctrl Pts',(182.415137827969,0.439989493930775,-103.889969301735));
#20450=CARTESIAN_POINT('Ctrl Pts',(182.477698497991,0.584280425728914,-104.2414573299));
#20451=CARTESIAN_POINT('Ctrl Pts',(182.489526917752,0.743827074166968,-104.557333471973));
#20452=CARTESIAN_POINT('Ctrl Pts',(181.69983365453,0.0076602008985784,-101.973943762289));
#20453=CARTESIAN_POINT('Ctrl Pts',(181.889202893271,0.0266495749489156,
-102.496369000122));
#20454=CARTESIAN_POINT('Ctrl Pts',(182.105417475816,0.132287381924616,-103.114033376099));
#20455=CARTESIAN_POINT('Ctrl Pts',(182.319938028905,0.390946554928068,-103.930656470914));
#20456=CARTESIAN_POINT('Ctrl Pts',(182.393341358782,0.530467074309935,-104.280008116939));
#20457=CARTESIAN_POINT('Ctrl Pts',(182.416553835504,0.687654147235085,-104.593350104552));
#20458=CARTESIAN_POINT('Ctrl Pts',(181.5749753816,0.000402959451920593,
-102.019536688494));
#20459=CARTESIAN_POINT('Ctrl Pts',(181.765769469498,0.0064585754895931,
-102.542012763284));
#20460=CARTESIAN_POINT('Ctrl Pts',(181.990548412461,0.0977146252752476,
-103.158388759139));
#20461=CARTESIAN_POINT('Ctrl Pts',(182.224838707103,0.341969925937946,-103.971322135667));
#20462=CARTESIAN_POINT('Ctrl Pts',(182.308539856551,0.47640526231532,-104.318648468817));
#20463=CARTESIAN_POINT('Ctrl Pts',(182.343580753256,0.631481220303202,-104.629366737131));
#20464=CARTESIAN_POINT('',(182.343580753256,0.631481220303021,-104.62936673713));
#20465=CARTESIAN_POINT('Origin',(182.4625,6.00000000000001,-101.95));
#20466=CARTESIAN_POINT('',(182.5625,3.10645162089483,-106.976666666667));
#20467=CARTESIAN_POINT('',(182.3625,3.00667409058086,-107.15));
#20468=CARTESIAN_POINT('',(182.5625,0.97333333333333,-104.843548379105));
#20469=CARTESIAN_POINT('Origin',(182.5625,6.00000000000001,-101.95));
#20470=CARTESIAN_POINT('',(182.5625,0.97333333333333,-104.843548379105));
#20471=CARTESIAN_POINT('Ctrl Pts',(182.5625,0.800000001098678,-104.521316839393));
#20472=CARTESIAN_POINT('Ctrl Pts',(182.5625,0.857236572714195,-104.634084947445));
#20473=CARTESIAN_POINT('Ctrl Pts',(182.5625,0.91490965910188,-104.742054884846));
#20474=CARTESIAN_POINT('Ctrl Pts',(182.5625,0.973333333333333,-104.843548379105));
#20475=CARTESIAN_POINT('Ctrl Pts',(182.489526917752,0.743827074166794,-104.557333471972));
#20476=CARTESIAN_POINT('Ctrl Pts',(182.49366244611,0.800286860789329,-104.669183196029));
#20477=CARTESIAN_POINT('Ctrl Pts',(182.495833333333,0.857713879611466,-104.77632510792));
#20478=CARTESIAN_POINT('Ctrl Pts',(182.495833333333,0.915555555555554,-104.876807555876));
#20479=CARTESIAN_POINT('Ctrl Pts',(182.416553835504,0.68765414723491,-104.593350104551));
#20480=CARTESIAN_POINT('Ctrl Pts',(182.42482489222,0.743337148864462,-104.704281444612));
#20481=CARTESIAN_POINT('Ctrl Pts',(182.429166666667,0.800518100121053,-104.810595330995));
#20482=CARTESIAN_POINT('Ctrl Pts',(182.429166666667,0.857777777777776,-104.910066732648));
#20483=CARTESIAN_POINT('Ctrl Pts',(182.343580753256,0.631481220303025,-104.62936673713));
#20484=CARTESIAN_POINT('Ctrl Pts',(182.355987338329,0.686387436939596,-104.739379693196));
#20485=CARTESIAN_POINT('Ctrl Pts',(182.3625,0.743322320630639,-104.844865554069));
#20486=CARTESIAN_POINT('Ctrl Pts',(182.3625,0.799999999999998,-104.943325909419));
#20487=CARTESIAN_POINT('Ctrl Pts',(182.5625,0.973333333333333,-104.843548379105));
#20488=CARTESIAN_POINT('Ctrl Pts',(182.5625,0.91490965910188,-104.742054884846));
#20489=CARTESIAN_POINT('Ctrl Pts',(182.5625,0.857236572714195,-104.634084947445));
#20490=CARTESIAN_POINT('Ctrl Pts',(182.5625,0.800000001098678,-104.521316839393));
#20491=CARTESIAN_POINT('Ctrl Pts',(182.5625,3.42868316199153,-107.149999999604));
#20492=CARTESIAN_POINT('Ctrl Pts',(182.562500000088,3.77824139277388,-107.327421746315));
#20493=CARTESIAN_POINT('Ctrl Pts',(182.504123937514,4.15716103788152,-107.487588700127));
#20494=CARTESIAN_POINT('Ctrl Pts',(182.295726889837,5.0552401086783,-107.780573645068));
#20495=CARTESIAN_POINT('Ctrl Pts',(182.122028319689,5.58142525423399,-107.886348035992));
#20496=CARTESIAN_POINT('Ctrl Pts',(181.949550265183,6.06724190764558,-107.927825300627));
#20497=CARTESIAN_POINT('Ctrl Pts',(182.489526917701,3.39266652940122,-107.206172926527));
#20498=CARTESIAN_POINT('Ctrl Pts',(182.476676711164,3.73937765477566,-107.381196742291));
#20499=CARTESIAN_POINT('Ctrl Pts',(182.407104407393,4.11610767175364,-107.535902098076));
#20500=CARTESIAN_POINT('Ctrl Pts',(182.178885909604,5.010573392444,-107.812220832665));
#20501=CARTESIAN_POINT('Ctrl Pts',(181.998732959996,5.5358352609817,-107.905551823336));
#20502=CARTESIAN_POINT('Ctrl Pts',(181.824691992404,6.02164898271766,-107.935082546577));
#20503=CARTESIAN_POINT('Ctrl Pts',(182.416553835402,3.3566498968109,-107.262345853449));
#20504=CARTESIAN_POINT('Ctrl Pts',(182.39094614805,3.70051482143434,-107.434941903931));
#20505=CARTESIAN_POINT('Ctrl Pts',(182.310082495261,4.07505274004195,-107.584215561193));
#20506=CARTESIAN_POINT('Ctrl Pts',(182.062102077776,4.96591130301164,-107.843861421252));
#20507=CARTESIAN_POINT('Ctrl Pts',(181.875666502886,5.49026758092219,-107.924762872177));
#20508=CARTESIAN_POINT('Ctrl Pts',(181.699833719625,5.97605605778975,-107.942339792527));
#20509=CARTESIAN_POINT('Ctrl Pts',(182.343580753104,3.32063326422059,-107.318518780371));
#20510=CARTESIAN_POINT('Ctrl Pts',(182.305122859126,3.66165108343612,-107.488716899907));
#20511=CARTESIAN_POINT('Ctrl Pts',(182.21306296514,4.03399937391406,-107.632528959141));
#20512=CARTESIAN_POINT('Ctrl Pts',(181.945261097542,4.92124458677734,-107.875508608848));
#20513=CARTESIAN_POINT('Ctrl Pts',(181.752371143193,5.4446775876699,-107.943966659521));
#20514=CARTESIAN_POINT('Ctrl Pts',(181.574975446846,5.93046313286183,-107.949597038478));
#20515=CARTESIAN_POINT('',(182.5625,3.42868316190269,-107.14999999978));
#20516=CARTESIAN_POINT('Ctrl Pts',(181.949550265183,6.06724190764558,-107.927825300627));
#20517=CARTESIAN_POINT('Ctrl Pts',(182.122028319689,5.58142525423399,-107.886348035992));
#20518=CARTESIAN_POINT('Ctrl Pts',(182.295726889837,5.0552401086783,-107.780573645068));
#20519=CARTESIAN_POINT('Ctrl Pts',(182.504123937514,4.15716103788152,-107.487588700127));
#20520=CARTESIAN_POINT('Ctrl Pts',(182.562500000088,3.77824139277388,-107.327421746315));
#20521=CARTESIAN_POINT('Ctrl Pts',(182.5625,3.42868316199153,-107.149999999604));
#20522=CARTESIAN_POINT('',(182.5625,3.42868316190269,-107.14999999978));
#20523=CARTESIAN_POINT('Ctrl Pts',(182.5625,3.10645162089484,-106.976666666667));
#20524=CARTESIAN_POINT('Ctrl Pts',(182.5625,3.21069598181732,-107.036673848678));
#20525=CARTESIAN_POINT('Ctrl Pts',(182.5625,3.3180193133645,-107.093831465749));
#20526=CARTESIAN_POINT('Ctrl Pts',(182.5625,3.42868316199166,-107.149999999604));
#20527=CARTESIAN_POINT('Ctrl Pts',(182.495833333333,3.07319244412351,-107.034444444444));
#20528=CARTESIAN_POINT('Ctrl Pts',(182.495833333333,3.17639835547358,-107.093853853762));
#20529=CARTESIAN_POINT('Ctrl Pts',(182.493585276875,3.28290392767116,-107.150766682816));
#20530=CARTESIAN_POINT('Ctrl Pts',(182.489526917701,3.39266652940134,-107.206172926527));
#20531=CARTESIAN_POINT('Ctrl Pts',(182.429166666667,3.03993326735219,-107.092222222222));
#20532=CARTESIAN_POINT('Ctrl Pts',(182.429166666667,3.14210072912985,-107.151033858845));
#20533=CARTESIAN_POINT('Ctrl Pts',(182.424670553749,3.24778854197781,-107.207701899883));
#20534=CARTESIAN_POINT('Ctrl Pts',(182.416553835402,3.35664989681103,-107.262345853449));
#20535=CARTESIAN_POINT('Ctrl Pts',(182.3625,3.00667409058087,-107.15));
#20536=CARTESIAN_POINT('Ctrl Pts',(182.3625,3.10780310278612,-107.208213863928));
#20537=CARTESIAN_POINT('Ctrl Pts',(182.355755830624,3.21267315628447,-107.26463711695));
#20538=CARTESIAN_POINT('Ctrl Pts',(182.343580753104,3.32063326422071,-107.318518780371));
#20539=CARTESIAN_POINT('Ctrl Pts',(182.5625,3.42868316199166,-107.149999999604));
#20540=CARTESIAN_POINT('Ctrl Pts',(182.5625,3.3180193133645,-107.093831465749));
#20541=CARTESIAN_POINT('Ctrl Pts',(182.5625,3.21069598181732,-107.036673848678));
#20542=CARTESIAN_POINT('Ctrl Pts',(182.5625,3.10645162089484,-106.976666666667));
#20543=CARTESIAN_POINT('Origin',(182.5625,63.5,-31.75));
#20544=CARTESIAN_POINT('',(182.5625,123.993325909419,-107.15));
#20545=CARTESIAN_POINT('',(182.5625,34.75,-107.15));
#20546=CARTESIAN_POINT('',(182.5625,126.2,-104.943325909419));
#20547=CARTESIAN_POINT('Origin',(182.5625,121.,-101.95));
#20548=CARTESIAN_POINT('',(182.5625,126.2,41.4433259094192));
#20549=CARTESIAN_POINT('',(182.5625,126.2,-66.85));
#20550=CARTESIAN_POINT('',(182.5625,123.993325909419,43.65));
#20551=CARTESIAN_POINT('Origin',(182.5625,121.,38.45));
#20552=CARTESIAN_POINT('',(182.5625,92.25,43.65));
#20553=CARTESIAN_POINT('Origin',(181.7625,34.75,-107.15));
#20554=CARTESIAN_POINT('',(181.7625,121.,-107.95));
#20555=CARTESIAN_POINT('',(181.7625,34.75,-107.95));
#20556=CARTESIAN_POINT('Ctrl Pts',(181.7625,121.,-107.95));
#20557=CARTESIAN_POINT('Ctrl Pts',(181.939990843115,121.486078692623,-107.95));
#20558=CARTESIAN_POINT('Ctrl Pts',(182.134486665857,122.014025751789,-107.887608349819));
#20559=CARTESIAN_POINT('Ctrl Pts',(182.444388077595,123.043713064318,-107.61628036626));
#20560=CARTESIAN_POINT('Ctrl Pts',(182.5625,123.544851663295,-107.408159534737));
#20561=CARTESIAN_POINT('Ctrl Pts',(182.5625,123.993325909419,-107.15));
#20562=CARTESIAN_POINT('Origin',(177.8,121.,-101.95));
#20563=CARTESIAN_POINT('',(178.6,121.,-107.95));
#20564=CARTESIAN_POINT('',(177.8,121.,-107.95));
#20565=CARTESIAN_POINT('Ctrl Pts',(177.8,123.993325909419,-107.15));
#20566=CARTESIAN_POINT('Ctrl Pts',(177.8,123.544851663295,-107.408159534737));
#20567=CARTESIAN_POINT('Ctrl Pts',(177.918111922405,123.043713064318,-107.61628036626));
#20568=CARTESIAN_POINT('Ctrl Pts',(178.228013334143,122.014025751789,-107.887608349819));
#20569=CARTESIAN_POINT('Ctrl Pts',(178.422509156885,121.486078692623,-107.95));
#20570=CARTESIAN_POINT('Ctrl Pts',(178.6,121.,-107.95));
#20571=CARTESIAN_POINT('',(178.6,127.,-101.95));
#20572=CARTESIAN_POINT('Ctrl Pts',(178.6,127.,-101.95));
#20573=CARTESIAN_POINT('Ctrl Pts',(178.422509156885,127.,-102.436078692623));
#20574=CARTESIAN_POINT('Ctrl Pts',(178.228013334143,126.937608349819,-102.964025751789));
#20575=CARTESIAN_POINT('Ctrl Pts',(177.918111922405,126.66628036626,-103.993713064318));
#20576=CARTESIAN_POINT('Ctrl Pts',(177.8,126.458159534737,-104.494851663295));
#20577=CARTESIAN_POINT('Ctrl Pts',(177.8,126.2,-104.943325909419));
#20578=CARTESIAN_POINT('',(181.7625,127.,-101.95));
#20579=CARTESIAN_POINT('',(177.8,127.,-101.95));
#20580=CARTESIAN_POINT('Ctrl Pts',(182.5625,126.2,-104.943325909419));
#20581=CARTESIAN_POINT('Ctrl Pts',(182.5625,126.458159534737,-104.494851663295));
#20582=CARTESIAN_POINT('Ctrl Pts',(182.444388077595,126.66628036626,-103.993713064318));
#20583=CARTESIAN_POINT('Ctrl Pts',(182.134486665857,126.937608349819,-102.964025751789));
#20584=CARTESIAN_POINT('Ctrl Pts',(181.939990843115,127.,-102.436078692623));
#20585=CARTESIAN_POINT('Ctrl Pts',(181.7625,127.,-101.95));
#20586=CARTESIAN_POINT('Origin',(177.8,6.,-107.95));
#20587=CARTESIAN_POINT('',(178.6,34.75,-107.95));
#20588=CARTESIAN_POINT('Origin',(178.6,34.75,-107.15));
#20589=CARTESIAN_POINT('Origin',(181.7625,126.2,-66.85));
#20590=CARTESIAN_POINT('',(181.7625,127.,38.45));
#20591=CARTESIAN_POINT('Ctrl Pts',(181.7625,127.,38.45));
#20592=CARTESIAN_POINT('Ctrl Pts',(181.939990843115,127.,38.9360786926232));
#20593=CARTESIAN_POINT('Ctrl Pts',(182.134486665857,126.937608349819,39.4640257517887));
#20594=CARTESIAN_POINT('Ctrl Pts',(182.444388077595,126.66628036626,40.4937130643181));
#20595=CARTESIAN_POINT('Ctrl Pts',(182.5625,126.458159534737,40.9948516632952));
#20596=CARTESIAN_POINT('Ctrl Pts',(182.5625,126.2,41.4433259094192));
#20597=CARTESIAN_POINT('',(181.7625,127.,-66.85));
#20598=CARTESIAN_POINT('Origin',(177.8,121.,38.45));
#20599=CARTESIAN_POINT('',(178.6,127.,38.45));
#20600=CARTESIAN_POINT('',(177.8,127.,38.45));
#20601=CARTESIAN_POINT('Ctrl Pts',(177.8,126.2,41.4433259094192));
#20602=CARTESIAN_POINT('Ctrl Pts',(177.8,126.458159534737,40.9948516632952));
#20603=CARTESIAN_POINT('Ctrl Pts',(177.918111922405,126.66628036626,40.4937130643181));
#20604=CARTESIAN_POINT('Ctrl Pts',(178.228013334143,126.937608349819,39.4640257517887));
#20605=CARTESIAN_POINT('Ctrl Pts',(178.422509156885,127.,38.9360786926232));
#20606=CARTESIAN_POINT('Ctrl Pts',(178.6,127.,38.45));
#20607=CARTESIAN_POINT('',(178.6,121.,44.45));
#20608=CARTESIAN_POINT('Ctrl Pts',(178.6,121.,44.45));
#20609=CARTESIAN_POINT('Ctrl Pts',(178.40913336376,121.52270981072,44.45));
#20610=CARTESIAN_POINT('Ctrl Pts',(178.182728070533,122.14501659934,44.3640989204313));
#20611=CARTESIAN_POINT('Ctrl Pts',(177.910747095178,123.089471451833,44.0921179450766));
#20612=CARTESIAN_POINT('Ctrl Pts',(177.8,123.591791866647,43.8811388949509));
#20613=CARTESIAN_POINT('Ctrl Pts',(177.8,123.993325909419,43.65));
#20614=CARTESIAN_POINT('',(181.7625,121.,44.45));
#20615=CARTESIAN_POINT('',(177.8,121.,44.45));
#20616=CARTESIAN_POINT('Ctrl Pts',(182.5625,123.993325909419,43.65));
#20617=CARTESIAN_POINT('Ctrl Pts',(182.5625,123.544851663295,43.9081595347366));
#20618=CARTESIAN_POINT('Ctrl Pts',(182.444388077595,123.043713064318,44.1162803662604));
#20619=CARTESIAN_POINT('Ctrl Pts',(182.134486665857,122.014025751789,44.387608349819));
#20620=CARTESIAN_POINT('Ctrl Pts',(181.939990843115,121.486078692623,44.45));
#20621=CARTESIAN_POINT('Ctrl Pts',(181.7625,121.,44.45));
#20622=CARTESIAN_POINT('Origin',(177.8,127.,-101.95));
#20623=CARTESIAN_POINT('',(178.6,127.,-66.85));
#20624=CARTESIAN_POINT('Origin',(178.6,126.2,-66.85));
#20625=CARTESIAN_POINT('Origin',(181.7625,92.25,43.65));
#20626=CARTESIAN_POINT('',(181.7625,92.25,44.45));
#20627=CARTESIAN_POINT('Origin',(177.8,121.,44.45));
#20628=CARTESIAN_POINT('',(178.6,92.25,44.45));
#20629=CARTESIAN_POINT('Origin',(178.6,92.25,43.65));
#20630=CARTESIAN_POINT('',(0.,0.,0.));
#20631=CARTESIAN_POINT('Ctrl Pts',(176.747537170301,126.999429809249,43.6801990080023));
#20632=CARTESIAN_POINT('Ctrl Pts',(176.745869694655,126.999493365079,43.678516554556));
#20633=CARTESIAN_POINT('Ctrl Pts',(176.733667226185,126.999932122919,43.6661745561527));
#20634=CARTESIAN_POINT('Ctrl Pts',(176.720285125676,126.999995921784,43.6526083802442));
#20635=CARTESIAN_POINT('Ctrl Pts',(176.718122408304,127.,43.6504214071384));
#20636=CARTESIAN_POINT('Ctrl Pts',(176.717705939749,127.,43.65));
#20637=CARTESIAN_POINT('Ctrl Pts',(176.841757782868,126.999429809249,43.5859783954351));
#20638=CARTESIAN_POINT('Ctrl Pts',(176.840085314622,126.999493365079,43.584300934589));
#20639=CARTESIAN_POINT('Ctrl Pts',(176.827829514792,126.999932122919,43.5720122675463));
#20640=CARTESIAN_POINT('Ctrl Pts',(176.814395290254,126.999995921784,43.5584982156664));
#20641=CARTESIAN_POINT('Ctrl Pts',(176.812222074582,127.,43.5563217408604));
#20642=CARTESIAN_POINT('Ctrl Pts',(176.811803959832,127.,43.5559019799162));
#20643=CARTESIAN_POINT('Ctrl Pts',(176.935978395435,126.999429809249,43.4917577828678));
#20644=CARTESIAN_POINT('Ctrl Pts',(176.934300934589,126.999493365079,43.490085314622));
#20645=CARTESIAN_POINT('Ctrl Pts',(176.921971487686,127.000007610143,43.4778295147916));
#20646=CARTESIAN_POINT('Ctrl Pts',(176.908492562627,126.999950474695,43.4643952902542));
#20647=CARTESIAN_POINT('Ctrl Pts',(176.90632174086,127.,43.4622220745824));
#20648=CARTESIAN_POINT('Ctrl Pts',(176.905901979916,127.,43.4618039598324));
#20649=CARTESIAN_POINT('Ctrl Pts',(177.030199008002,126.999429809249,43.3975371703006));
#20650=CARTESIAN_POINT('Ctrl Pts',(177.028516554556,126.999493365079,43.395869694655));
#20651=CARTESIAN_POINT('Ctrl Pts',(177.016174556153,126.999932122919,43.3836672261852));
#20652=CARTESIAN_POINT('Ctrl Pts',(177.002608380244,126.999995921784,43.3702851256763));
#20653=CARTESIAN_POINT('Ctrl Pts',(177.000421407138,127.,43.3681224083043));
#20654=CARTESIAN_POINT('Ctrl Pts',(177.,127.,43.3677059397485));
#20655=CARTESIAN_POINT('',(176.717705939749,127.,43.65));
#20656=CARTESIAN_POINT('',(176.747537170301,126.999429809249,43.6801990080023));
#20657=CARTESIAN_POINT('Ctrl Pts',(176.717705939749,127.,43.65));
#20658=CARTESIAN_POINT('Ctrl Pts',(176.717872698805,127.,43.650168736525));
#20659=CARTESIAN_POINT('Ctrl Pts',(176.718042672762,126.999999960859,43.6503407294752));
#20660=CARTESIAN_POINT('Ctrl Pts',(176.718271119852,126.999999795533,43.6505719684178));
#20661=CARTESIAN_POINT('Ctrl Pts',(176.718523239385,126.999999613074,43.6508271691041));
#20662=CARTESIAN_POINT('Ctrl Pts',(176.718846507485,126.99999928102,43.6511544591101));
#20663=CARTESIAN_POINT('Ctrl Pts',(176.719268262893,126.999998436683,43.6515815512717));
#20664=CARTESIAN_POINT('Ctrl Pts',(176.719739279202,126.999997493728,43.6520585276647));
#20665=CARTESIAN_POINT('Ctrl Pts',(176.720332661821,126.999995895344,43.6526595049513));
#20666=CARTESIAN_POINT('Ctrl Pts',(176.721034596213,126.999992899769,43.6533705073352));
#20667=CARTESIAN_POINT('Ctrl Pts',(176.721922356591,126.999989111163,43.654269736312));
#20668=CARTESIAN_POINT('Ctrl Pts',(176.72298234306,126.999982983391,43.6553435322326));
#20669=CARTESIAN_POINT('Ctrl Pts',(176.724119373636,126.999973630094,43.6564954718405));
#20670=CARTESIAN_POINT('Ctrl Pts',(176.725267024347,126.999964189434,43.6576581708371));
#20671=CARTESIAN_POINT('Ctrl Pts',(176.726487764087,126.999951463521,43.6588950097938));
#20672=CARTESIAN_POINT('Ctrl Pts',(176.727682323414,126.999936173481,43.6601053627628));
#20673=CARTESIAN_POINT('Ctrl Pts',(176.728576869224,126.999924723534,43.6610117356424));
#20674=CARTESIAN_POINT('Ctrl Pts',(176.729456205746,126.999911911841,43.6619027203553));
#20675=CARTESIAN_POINT('Ctrl Pts',(176.730305951649,126.999898173663,43.6627636895374));
#20676=CARTESIAN_POINT('Ctrl Pts',(176.731077458531,126.999885700406,43.6635453863343));
#20677=CARTESIAN_POINT('Ctrl Pts',(176.731824182401,126.999872502733,43.6643019452847));
#20678=CARTESIAN_POINT('Ctrl Pts',(176.732566882097,126.999858342121,43.665054319646));
#20679=CARTESIAN_POINT('Ctrl Pts',(176.733343831679,126.999843528486,43.6658413900453));
#20680=CARTESIAN_POINT('Ctrl Pts',(176.734123555715,126.99982752742,43.6666311424732));
#20681=CARTESIAN_POINT('Ctrl Pts',(176.734930805536,126.999809694323,43.6674485777798));
#20682=CARTESIAN_POINT('Ctrl Pts',(176.735832024149,126.999789785346,43.6683611675309));
#20683=CARTESIAN_POINT('Ctrl Pts',(176.736766994247,126.999767552882,43.6693076969592));
#20684=CARTESIAN_POINT('Ctrl Pts',(176.737717360141,126.999743173977,43.670269575142));
#20685=CARTESIAN_POINT('Ctrl Pts',(176.738959763474,126.999711303693,43.6715270283689));
#20686=CARTESIAN_POINT('Ctrl Pts',(176.740226781866,126.999675666215,43.6728089911326));
#20687=CARTESIAN_POINT('Ctrl Pts',(176.741404811927,126.999639900927,43.6740006009478));
#20688=CARTESIAN_POINT('Ctrl Pts',(176.742367569254,126.999610671373,43.6749744564707));
#20689=CARTESIAN_POINT('Ctrl Pts',(176.743267661294,126.999581516184,43.6758847018519));
#20690=CARTESIAN_POINT('Ctrl Pts',(176.744045268374,126.999555290462,43.6766709110228));
#20691=CARTESIAN_POINT('Ctrl Pts',(176.744722380664,126.999532454046,43.6773555137054));
#20692=CARTESIAN_POINT('Ctrl Pts',(176.745305724149,126.999511912239,43.6779451634335));
#20693=CARTESIAN_POINT('Ctrl Pts',(176.745779966788,126.999494873465,43.6784244138591));
#20694=CARTESIAN_POINT('Ctrl Pts',(176.746218303809,126.999479124722,43.6788673795207));
#20695=CARTESIAN_POINT('Ctrl Pts',(176.746562942419,126.999466401456,43.6792155329358));
#20696=CARTESIAN_POINT('Ctrl Pts',(176.746832907361,126.999456345864,43.6794881511433));
#20697=CARTESIAN_POINT('Ctrl Pts',(176.747083726891,126.999447003396,43.6797414357741));
#20698=CARTESIAN_POINT('Ctrl Pts',(176.74726987331,126.999439970325,43.6799293013882));
#20699=CARTESIAN_POINT('Ctrl Pts',(176.747439207675,126.999433537031,43.6801001639586));
#20700=CARTESIAN_POINT('Ctrl Pts',(176.747472215255,126.999432283018,43.6801334694242));
#20701=CARTESIAN_POINT('Ctrl Pts',(176.747504695246,126.999431047036,43.6801662412462));
#20702=CARTESIAN_POINT('Ctrl Pts',(176.747537170301,126.999429809249,43.6801990080023));
#20703=CARTESIAN_POINT('',(177.030199008002,126.999429809249,43.3975371703006));
#20704=CARTESIAN_POINT('Ctrl Pts',(177.030199008002,126.999429809249,43.3975371703006));
#20705=CARTESIAN_POINT('Ctrl Pts',(176.935978395435,126.999429809249,43.4917577828678));
#20706=CARTESIAN_POINT('Ctrl Pts',(176.841757782868,126.999429809249,43.5859783954351));
#20707=CARTESIAN_POINT('Ctrl Pts',(176.747537170301,126.999429809249,43.6801990080023));
#20708=CARTESIAN_POINT('',(177.,127.,43.3677059397485));
#20709=CARTESIAN_POINT('Ctrl Pts',(177.030199008002,126.999429809249,43.3975371703006));
#20710=CARTESIAN_POINT('Ctrl Pts',(177.030030585505,126.999436171524,43.3973702471606));
#20711=CARTESIAN_POINT('Ctrl Pts',(177.029858909386,126.999442617638,43.3972001071489));
#20712=CARTESIAN_POINT('Ctrl Pts',(177.029628057339,126.99945117313,43.396971463311));
#20713=CARTESIAN_POINT('Ctrl Pts',(177.029373282892,126.999460615197,43.3967191259022));
#20714=CARTESIAN_POINT('Ctrl Pts',(177.029046504163,126.999472627869,43.3963956021262));
#20715=CARTESIAN_POINT('Ctrl Pts',(177.028620026165,126.999487894907,43.395973543409));
#20716=CARTESIAN_POINT('Ctrl Pts',(177.0281437326,126.999504945239,43.3955021853265));
#20717=CARTESIAN_POINT('Ctrl Pts',(177.027543563761,126.999526020176,43.3949084001559));
#20718=CARTESIAN_POINT('Ctrl Pts',(177.026833440411,126.999549852402,43.394206022241));
#20719=CARTESIAN_POINT('Ctrl Pts',(177.025935290825,126.999579994917,43.3933176689235));
#20720=CARTESIAN_POINT('Ctrl Pts',(177.0248626695,126.999614390365,43.3922570121512));
#20721=CARTESIAN_POINT('Ctrl Pts',(177.023711822739,126.999648516201,43.3911193310076));
#20722=CARTESIAN_POINT('Ctrl Pts',(177.02255032393,126.9996829579,43.3899711196752));
#20723=CARTESIAN_POINT('Ctrl Pts',(177.021314608223,126.999716919438,43.3887498553891));
#20724=CARTESIAN_POINT('Ctrl Pts',(177.02010513109,126.999747324912,43.3875548864531));
#20725=CARTESIAN_POINT('Ctrl Pts',(177.019199401769,126.999770094362,43.3866600217438));
#20726=CARTESIAN_POINT('Ctrl Pts',(177.018308923963,126.999790925398,43.3857804315058));
#20727=CARTESIAN_POINT('Ctrl Pts',(177.017448288609,126.999809700632,43.384930519969));
#20728=CARTESIAN_POINT('Ctrl Pts',(177.016666887984,126.999826747316,43.3841588558682));
#20729=CARTESIAN_POINT('Ctrl Pts',(177.015910483889,126.999842123653,43.3834120480744));
#20730=CARTESIAN_POINT('Ctrl Pts',(177.015158111381,126.999856381896,43.3826693398961));
#20731=CARTESIAN_POINT('Ctrl Pts',(177.014371053415,126.999871297464,43.3818923917999));
#20732=CARTESIAN_POINT('Ctrl Pts',(177.013581145567,126.999885130105,43.3811127516123));
#20733=CARTESIAN_POINT('Ctrl Pts',(177.012763400092,126.999898178282,43.3803056659763));
#20734=CARTESIAN_POINT('Ctrl Pts',(177.011850452589,126.999912745528,43.3794046193326));
#20735=CARTESIAN_POINT('Ctrl Pts',(177.010903370168,126.999926273619,43.3784699201045));
#20736=CARTESIAN_POINT('Ctrl Pts',(177.00994078853,126.999938235568,43.3775198964634));
#20737=CARTESIAN_POINT('Ctrl Pts',(177.008682347624,126.999953874144,43.3762778733826));
#20738=CARTESIAN_POINT('Ctrl Pts',(177.007399134253,126.999966671765,43.375011353504));
#20739=CARTESIAN_POINT('Ctrl Pts',(177.006206223417,126.999975926382,43.3738338670282));
#20740=CARTESIAN_POINT('Ctrl Pts',(177.00523142736,126.999983488862,43.3728716751026));
#20741=CARTESIAN_POINT('Ctrl Pts',(177.004320197324,126.999988722094,43.3719721616102));
#20742=CARTESIAN_POINT('Ctrl Pts',(177.003533069758,126.999992198348,43.3711950841717));
#20743=CARTESIAN_POINT('Ctrl Pts',(177.002847649353,126.999995225425,43.3705184152863));
#20744=CARTESIAN_POINT('Ctrl Pts',(177.002257239447,126.999996959481,43.3699354824491));
#20745=CARTESIAN_POINT('Ctrl Pts',(177.001777334972,126.999998025673,43.369461595752));
#20746=CARTESIAN_POINT('Ctrl Pts',(177.00133376131,126.999999011149,43.3690235842967));
#20747=CARTESIAN_POINT('Ctrl Pts',(177.000985093106,126.999999440092,43.3686792256923));
#20748=CARTESIAN_POINT('Ctrl Pts',(177.000712044094,126.999999683121,43.368409497874));
#20749=CARTESIAN_POINT('Ctrl Pts',(177.000458357712,126.999999908916,43.3681588971718));
#20750=CARTESIAN_POINT('Ctrl Pts',(177.000270163794,126.999999972695,43.3679729332256));
#20751=CARTESIAN_POINT('Ctrl Pts',(177.000098987777,126.999999993876,43.3678037667735));
#20752=CARTESIAN_POINT('Ctrl Pts',(177.000065634447,126.999999998003,43.3677708050029));
#20753=CARTESIAN_POINT('Ctrl Pts',(177.000032814729,127.,43.3677383699128));
#20754=CARTESIAN_POINT('Ctrl Pts',(177.,127.,43.3677059397485));
#20755=CARTESIAN_POINT('',(176.858852969874,127.,43.5088529698743));
#20756=CARTESIAN_POINT('Ctrl Pts',(177.030199008002,122.238070190751,43.3975371703006));
#20757=CARTESIAN_POINT('Ctrl Pts',(177.028516554556,122.238006634921,43.395869694655));
#20758=CARTESIAN_POINT('Ctrl Pts',(177.016174465217,122.237567875321,43.3836671357425));
#20759=CARTESIAN_POINT('Ctrl Pts',(177.002608356514,122.237504077912,43.3702851021113));
#20760=CARTESIAN_POINT('Ctrl Pts',(177.000421407138,122.2375,43.3681224083044));
#20761=CARTESIAN_POINT('Ctrl Pts',(177.,122.2375,43.3677059397486));
#20762=CARTESIAN_POINT('Ctrl Pts',(176.935978395435,122.238070190751,43.4917577828679));
#20763=CARTESIAN_POINT('Ctrl Pts',(176.934300934589,122.238006634921,43.490085314622));
#20764=CARTESIAN_POINT('Ctrl Pts',(176.92201217661,122.237567875321,43.4778294243489));
#20765=CARTESIAN_POINT('Ctrl Pts',(176.908498191936,122.237504077912,43.4643952666892));
#20766=CARTESIAN_POINT('Ctrl Pts',(176.90632174086,122.2375,43.4622220745824));
#20767=CARTESIAN_POINT('Ctrl Pts',(176.905901979916,122.2375,43.4618039598324));
#20768=CARTESIAN_POINT('Ctrl Pts',(176.841757782868,122.238070190751,43.5859783954351));
#20769=CARTESIAN_POINT('Ctrl Pts',(176.840085314622,122.238006634921,43.5843009345891));
#20770=CARTESIAN_POINT('Ctrl Pts',(176.827829424349,122.237492398776,43.571971396334));
#20771=CARTESIAN_POINT('Ctrl Pts',(176.814395266689,122.237549527789,43.5584925388249));
#20772=CARTESIAN_POINT('Ctrl Pts',(176.812222074582,122.2375,43.5563217408604));
#20773=CARTESIAN_POINT('Ctrl Pts',(176.811803959832,122.2375,43.5559019799162));
#20774=CARTESIAN_POINT('Ctrl Pts',(176.747537170301,122.238070190751,43.6801990080024));
#20775=CARTESIAN_POINT('Ctrl Pts',(176.745869694655,122.238006634921,43.6785165545561));
#20776=CARTESIAN_POINT('Ctrl Pts',(176.733667135743,122.237567875321,43.6661744652167));
#20777=CARTESIAN_POINT('Ctrl Pts',(176.720285102111,122.237504077912,43.6526083565139));
#20778=CARTESIAN_POINT('Ctrl Pts',(176.718122408304,122.2375,43.6504214071384));
#20779=CARTESIAN_POINT('Ctrl Pts',(176.717705939749,122.2375,43.65));
#20780=CARTESIAN_POINT('',(177.,122.2375,43.3677059397486));
#20781=CARTESIAN_POINT('',(177.030199008002,122.238070190751,43.3975371703006));
#20782=CARTESIAN_POINT('Ctrl Pts',(177.,122.2375,43.3677059397486));
#20783=CARTESIAN_POINT('Ctrl Pts',(177.000168736525,122.2375,43.3678726988053));
#20784=CARTESIAN_POINT('Ctrl Pts',(177.000340729475,122.237500039141,43.3680426727623));
#20785=CARTESIAN_POINT('Ctrl Pts',(177.000571968418,122.237500204467,43.3682711198523));
#20786=CARTESIAN_POINT('Ctrl Pts',(177.000827169104,122.237500386926,43.3685232393849));
#20787=CARTESIAN_POINT('Ctrl Pts',(177.00115445911,122.23750071898,43.3688465074852));
#20788=CARTESIAN_POINT('Ctrl Pts',(177.001581551272,122.237501563317,43.3692682628933));
#20789=CARTESIAN_POINT('Ctrl Pts',(177.002058527665,122.237502506272,43.3697392792016));
#20790=CARTESIAN_POINT('Ctrl Pts',(177.002659504951,122.237504104656,43.3703326618207));
#20791=CARTESIAN_POINT('Ctrl Pts',(177.003370507335,122.237507100231,43.3710345962129));
#20792=CARTESIAN_POINT('Ctrl Pts',(177.004269736312,122.237510888837,43.3719223565912));
#20793=CARTESIAN_POINT('Ctrl Pts',(177.005343532233,122.237517016609,43.3729823430604));
#20794=CARTESIAN_POINT('Ctrl Pts',(177.006495471841,122.237526369906,43.3741193736364));
#20795=CARTESIAN_POINT('Ctrl Pts',(177.007658170837,122.237535810566,43.3752670243474));
#20796=CARTESIAN_POINT('Ctrl Pts',(177.008895009794,122.237548536479,43.3764877640871));
#20797=CARTESIAN_POINT('Ctrl Pts',(177.010105362763,122.237563826519,43.3776823234142));
#20798=CARTESIAN_POINT('Ctrl Pts',(177.011011735643,122.237575276466,43.3785768692244));
#20799=CARTESIAN_POINT('Ctrl Pts',(177.011902720356,122.237588088159,43.3794562057466));
#20800=CARTESIAN_POINT('Ctrl Pts',(177.012763689538,122.237601826337,43.3803059516489));
#20801=CARTESIAN_POINT('Ctrl Pts',(177.013545386334,122.237614299594,43.3810774585317));
#20802=CARTESIAN_POINT('Ctrl Pts',(177.014301945285,122.237627497267,43.3818241824014));
#20803=CARTESIAN_POINT('Ctrl Pts',(177.015054319646,122.237641657879,43.3825668820968));
#20804=CARTESIAN_POINT('Ctrl Pts',(177.015841390045,122.237656471514,43.3833438316793));
#20805=CARTESIAN_POINT('Ctrl Pts',(177.016631142473,122.23767247258,43.3841235557154));
#20806=CARTESIAN_POINT('Ctrl Pts',(177.01744857778,122.237690305677,43.3849308055361));
#20807=CARTESIAN_POINT('Ctrl Pts',(177.018361167531,122.237710214654,43.3858320241488));
#20808=CARTESIAN_POINT('Ctrl Pts',(177.019307696959,122.237732447118,43.3867669942467));
#20809=CARTESIAN_POINT('Ctrl Pts',(177.020269575142,122.237756826022,43.3877173601411));
#20810=CARTESIAN_POINT('Ctrl Pts',(177.021527028369,122.237788696307,43.3889597634745));
#20811=CARTESIAN_POINT('Ctrl Pts',(177.022808991133,122.237824333785,43.390226781866));
#20812=CARTESIAN_POINT('Ctrl Pts',(177.024000600948,122.237860099073,43.3914048119272));
#20813=CARTESIAN_POINT('Ctrl Pts',(177.024974456471,122.237889328627,43.3923675692547));
#20814=CARTESIAN_POINT('Ctrl Pts',(177.025884701852,122.237918483816,43.3932676612944));
#20815=CARTESIAN_POINT('Ctrl Pts',(177.026670911023,122.237944709538,43.394045268374));
#20816=CARTESIAN_POINT('Ctrl Pts',(177.027355513706,122.237967545954,43.3947223806646));
#20817=CARTESIAN_POINT('Ctrl Pts',(177.027945163434,122.237988087761,43.3953057241498));
#20818=CARTESIAN_POINT('Ctrl Pts',(177.028424413859,122.238005126535,43.395779966788));
#20819=CARTESIAN_POINT('Ctrl Pts',(177.028867379521,122.238020875278,43.3962183038092));
#20820=CARTESIAN_POINT('Ctrl Pts',(177.029215532936,122.238033598544,43.3965629424196));
#20821=CARTESIAN_POINT('Ctrl Pts',(177.029488151143,122.238043654136,43.3968329073614));
#20822=CARTESIAN_POINT('Ctrl Pts',(177.029741435774,122.238052996604,43.3970837268911));
#20823=CARTESIAN_POINT('Ctrl Pts',(177.029929301388,122.238060029675,43.3972698733102));
#20824=CARTESIAN_POINT('Ctrl Pts',(177.030100163959,122.238066462969,43.3974392076751));
#20825=CARTESIAN_POINT('Ctrl Pts',(177.030133469424,122.238067716982,43.3974722152546));
#20826=CARTESIAN_POINT('Ctrl Pts',(177.030166241246,122.238068952964,43.3975046952459));
#20827=CARTESIAN_POINT('Ctrl Pts',(177.030199008002,122.238070190751,43.3975371703006));
#20828=CARTESIAN_POINT('',(176.747537170301,122.238070190751,43.6801990080024));
#20829=CARTESIAN_POINT('Ctrl Pts',(176.747537170301,122.238070190751,43.6801990080024));
#20830=CARTESIAN_POINT('Ctrl Pts',(176.841757782868,122.238070190751,43.5859783954351));
#20831=CARTESIAN_POINT('Ctrl Pts',(176.935978395435,122.238070190751,43.4917577828679));
#20832=CARTESIAN_POINT('Ctrl Pts',(177.030199008002,122.238070190751,43.3975371703006));
#20833=CARTESIAN_POINT('',(176.717705939749,122.2375,43.65));
#20834=CARTESIAN_POINT('Ctrl Pts',(176.747537170301,122.238070190751,43.6801990080024));
#20835=CARTESIAN_POINT('Ctrl Pts',(176.747370247161,122.238063828476,43.6800305855052));
#20836=CARTESIAN_POINT('Ctrl Pts',(176.747200107149,122.238057382362,43.6798589093858));
#20837=CARTESIAN_POINT('Ctrl Pts',(176.746971463311,122.23804882687,43.6796280573389));
#20838=CARTESIAN_POINT('Ctrl Pts',(176.746719125902,122.238039384803,43.679373282892));
#20839=CARTESIAN_POINT('Ctrl Pts',(176.746395602126,122.238027372131,43.6790465041629));
#20840=CARTESIAN_POINT('Ctrl Pts',(176.745973543409,122.238012105093,43.6786200261655));
#20841=CARTESIAN_POINT('Ctrl Pts',(176.745502185327,122.237995054761,43.6781437326003));
#20842=CARTESIAN_POINT('Ctrl Pts',(176.744908400156,122.237973979824,43.6775435637607));
#20843=CARTESIAN_POINT('Ctrl Pts',(176.744206022241,122.237950147598,43.6768334404111));
#20844=CARTESIAN_POINT('Ctrl Pts',(176.743317668924,122.237920005083,43.6759352908253));
#20845=CARTESIAN_POINT('Ctrl Pts',(176.742257012151,122.237885609635,43.6748626694999));
#20846=CARTESIAN_POINT('Ctrl Pts',(176.741119331008,122.237851483799,43.6737118227386));
#20847=CARTESIAN_POINT('Ctrl Pts',(176.739971119675,122.2378170421,43.6725503239298));
#20848=CARTESIAN_POINT('Ctrl Pts',(176.738749855389,122.237783080562,43.6713146082227));
#20849=CARTESIAN_POINT('Ctrl Pts',(176.737554886453,122.237752675088,43.67010513109));
#20850=CARTESIAN_POINT('Ctrl Pts',(176.736660021744,122.237729905638,43.6691994017693));
#20851=CARTESIAN_POINT('Ctrl Pts',(176.735780431506,122.237709074602,43.6683089239629));
#20852=CARTESIAN_POINT('Ctrl Pts',(176.734930519969,122.237690299368,43.6674482886094));
#20853=CARTESIAN_POINT('Ctrl Pts',(176.734158855873,122.237673252684,43.6666668879893));
#20854=CARTESIAN_POINT('Ctrl Pts',(176.733412048084,122.237657876347,43.6659104838988));
#20855=CARTESIAN_POINT('Ctrl Pts',(176.73266933991,122.237643618104,43.665158111395));
#20856=CARTESIAN_POINT('Ctrl Pts',(176.731892391814,122.237628702536,43.6643710534291));
#20857=CARTESIAN_POINT('Ctrl Pts',(176.731112751627,122.237614869895,43.6635811455825));
#20858=CARTESIAN_POINT('Ctrl Pts',(176.730305665992,122.237601821719,43.6627634001078));
#20859=CARTESIAN_POINT('Ctrl Pts',(176.729404619349,122.237587254472,43.6618504526061));
#20860=CARTESIAN_POINT('Ctrl Pts',(176.728469920122,122.237573726382,43.6609033701865));
#20861=CARTESIAN_POINT('Ctrl Pts',(176.727519896482,122.237561764432,43.6599407885492));
#20862=CARTESIAN_POINT('Ctrl Pts',(176.726277873407,122.237546125856,43.6586823476483));
#20863=CARTESIAN_POINT('Ctrl Pts',(176.725011353533,122.237533328236,43.6573991342823));
#20864=CARTESIAN_POINT('Ctrl Pts',(176.723833867061,122.237524073618,43.6562062234503));
#20865=CARTESIAN_POINT('Ctrl Pts',(176.722871675132,122.237516511138,43.6552314273898));
#20866=CARTESIAN_POINT('Ctrl Pts',(176.721972161636,122.237511277906,43.6543201973493));
#20867=CARTESIAN_POINT('Ctrl Pts',(176.721195084193,122.237507801652,43.6535330697796));
#20868=CARTESIAN_POINT('Ctrl Pts',(176.720518415305,122.237504774575,43.6528476493719));
#20869=CARTESIAN_POINT('Ctrl Pts',(176.719935482465,122.237503040519,43.6522572394634));
#20870=CARTESIAN_POINT('Ctrl Pts',(176.719461595766,122.237501974327,43.6517773349856));
#20871=CARTESIAN_POINT('Ctrl Pts',(176.719023584308,122.237500988851,43.6513337613213));
#20872=CARTESIAN_POINT('Ctrl Pts',(176.718679225702,122.237500559908,43.6509850931152));
#20873=CARTESIAN_POINT('Ctrl Pts',(176.718409497882,122.237500316879,43.6507120441015));
#20874=CARTESIAN_POINT('Ctrl Pts',(176.718158897178,122.237500091084,43.6504583577189));
#20875=CARTESIAN_POINT('Ctrl Pts',(176.717972933231,122.237500027304,43.6502701637992));
#20876=CARTESIAN_POINT('Ctrl Pts',(176.717803766779,122.237500006124,43.6500989877827));
#20877=CARTESIAN_POINT('Ctrl Pts',(176.717770805006,122.237500001997,43.6500656344504));
#20878=CARTESIAN_POINT('Ctrl Pts',(176.717738369915,122.2375,43.6500328147306));
#20879=CARTESIAN_POINT('Ctrl Pts',(176.717705939749,122.2375,43.65));
#20880=CARTESIAN_POINT('',(176.858852969874,122.2375,43.5088529698743));
#20881=CARTESIAN_POINT('Ctrl Pts',(176.747537170301,122.238070190751,43.6801990080024));
#20882=CARTESIAN_POINT('Ctrl Pts',(176.878145139865,122.243048313183,43.8119801402103));
#20883=CARTESIAN_POINT('Ctrl Pts',(177.142745845888,122.319065602083,44.0669582028244));
#20884=CARTESIAN_POINT('Ctrl Pts',(177.429161451671,122.559475348238,44.3164670343898));
#20885=CARTESIAN_POINT('Ctrl Pts',(177.574122249711,122.816490807511,44.43105315404));
#20886=CARTESIAN_POINT('Ctrl Pts',(177.6,122.964234224196,44.45));
#20887=CARTESIAN_POINT('Ctrl Pts',(177.6,123.0375,44.45));
#20888=CARTESIAN_POINT('Ctrl Pts',(176.841757782868,122.238070190751,43.5859783954351));
#20889=CARTESIAN_POINT('Ctrl Pts',(176.972756806647,122.243048313183,43.7173684734285));
#20890=CARTESIAN_POINT('Ctrl Pts',(177.234149964867,122.319065602083,43.9755540838455));
#20891=CARTESIAN_POINT('Ctrl Pts',(177.508263312577,122.559475348238,44.2373651734836));
#20892=CARTESIAN_POINT('Ctrl Pts',(177.643099217821,122.816490807511,44.3620761859304));
#20893=CARTESIAN_POINT('Ctrl Pts',(177.666666666667,122.964234224196,44.3833333333333));
#20894=CARTESIAN_POINT('Ctrl Pts',(177.666666666667,123.0375,44.3833333333333));
#20895=CARTESIAN_POINT('Ctrl Pts',(176.935978395435,122.238070190751,43.4917577828679));
#20896=CARTESIAN_POINT('Ctrl Pts',(177.067368473429,122.243048313183,43.6227568066467));
#20897=CARTESIAN_POINT('Ctrl Pts',(177.325554083845,122.319065602083,43.8841499648667));
#20898=CARTESIAN_POINT('Ctrl Pts',(177.587365173484,122.559475348238,44.1582633125774));
#20899=CARTESIAN_POINT('Ctrl Pts',(177.71207618593,122.816490807511,44.2930992178208));
#20900=CARTESIAN_POINT('Ctrl Pts',(177.733333333333,122.964234224196,44.3166666666667));
#20901=CARTESIAN_POINT('Ctrl Pts',(177.733333333333,123.0375,44.3166666666667));
#20902=CARTESIAN_POINT('Ctrl Pts',(177.030199008002,122.238070190751,43.3975371703006));
#20903=CARTESIAN_POINT('Ctrl Pts',(177.16198014021,122.243048313183,43.5281451398648));
#20904=CARTESIAN_POINT('Ctrl Pts',(177.416958202824,122.319065602083,43.7927458458878));
#20905=CARTESIAN_POINT('Ctrl Pts',(177.66646703439,122.559475348238,44.0791614516713));
#20906=CARTESIAN_POINT('Ctrl Pts',(177.78105315404,122.816490807511,44.2241222497112));
#20907=CARTESIAN_POINT('Ctrl Pts',(177.8,122.964234224196,44.25));
#20908=CARTESIAN_POINT('Ctrl Pts',(177.8,123.0375,44.25));
#20909=CARTESIAN_POINT('',(177.8,123.0375,44.25));
#20910=CARTESIAN_POINT('Ctrl Pts',(177.030199008002,122.238070190751,43.3975371703006));
#20911=CARTESIAN_POINT('Ctrl Pts',(177.16198014021,122.243048313183,43.5281451398648));
#20912=CARTESIAN_POINT('Ctrl Pts',(177.416958202824,122.319065602083,43.7927458458878));
#20913=CARTESIAN_POINT('Ctrl Pts',(177.66646703439,122.559475348238,44.0791614516713));
#20914=CARTESIAN_POINT('Ctrl Pts',(177.78105315404,122.816490807511,44.2241222497112));
#20915=CARTESIAN_POINT('Ctrl Pts',(177.8,122.964234224196,44.25));
#20916=CARTESIAN_POINT('Ctrl Pts',(177.8,123.0375,44.25));
#20917=CARTESIAN_POINT('',(177.6,123.0375,44.45));
#20918=CARTESIAN_POINT('',(177.8,123.0375,44.25));
#20919=CARTESIAN_POINT('Ctrl Pts',(177.6,123.0375,44.45));
#20920=CARTESIAN_POINT('Ctrl Pts',(177.6,122.964234224196,44.45));
#20921=CARTESIAN_POINT('Ctrl Pts',(177.574122249711,122.816490807511,44.43105315404));
#20922=CARTESIAN_POINT('Ctrl Pts',(177.429161451671,122.559475348238,44.3164670343898));
#20923=CARTESIAN_POINT('Ctrl Pts',(177.142745845888,122.319065602083,44.0669582028244));
#20924=CARTESIAN_POINT('Ctrl Pts',(176.878145139865,122.243048313183,43.8119801402103));
#20925=CARTESIAN_POINT('Ctrl Pts',(176.747537170301,122.238070190751,43.6801990080024));
#20926=CARTESIAN_POINT('Origin',(177.7,122.2375,44.35));
#20927=CARTESIAN_POINT('',(177.8,126.2,44.25));
#20928=CARTESIAN_POINT('',(177.6,126.2,44.45));
#20929=CARTESIAN_POINT('',(177.8,126.2,44.25));
#20930=CARTESIAN_POINT('',(177.6,122.2375,44.45));
#20931=CARTESIAN_POINT('',(177.8,122.2375,44.25));
#20932=CARTESIAN_POINT('Ctrl Pts',(177.030199008002,126.999429809249,43.3975371703006));
#20933=CARTESIAN_POINT('Ctrl Pts',(177.227870706314,126.991962625601,43.5934491246469));
#20934=CARTESIAN_POINT('Ctrl Pts',(177.539136404472,126.85217227369,43.9258693224329));
#20935=CARTESIAN_POINT('Ctrl Pts',(177.766798305442,126.497803729337,44.2039283446181));
#20936=CARTESIAN_POINT('Ctrl Pts',(177.8,126.297687701072,44.25));
#20937=CARTESIAN_POINT('Ctrl Pts',(177.8,126.2,44.25));
#20938=CARTESIAN_POINT('Ctrl Pts',(176.935978395435,126.999429809249,43.4917577828678));
#20939=CARTESIAN_POINT('Ctrl Pts',(177.133063512425,126.991962625601,43.688256318536));
#20940=CARTESIAN_POINT('Ctrl Pts',(177.451380710459,126.85217227369,44.0136250164458));
#20941=CARTESIAN_POINT('Ctrl Pts',(177.695841651834,126.497803729337,44.274884998226));
#20942=CARTESIAN_POINT('Ctrl Pts',(177.733333333333,126.297687701072,44.3166666666667));
#20943=CARTESIAN_POINT('Ctrl Pts',(177.733333333333,126.2,44.3166666666667));
#20944=CARTESIAN_POINT('Ctrl Pts',(176.841757782868,126.999429809249,43.5859783954351));
#20945=CARTESIAN_POINT('Ctrl Pts',(177.038256318536,126.991962625601,43.7830635124252));
#20946=CARTESIAN_POINT('Ctrl Pts',(177.363625016446,126.85217227369,44.1013807104587));
#20947=CARTESIAN_POINT('Ctrl Pts',(177.624884998226,126.497803729337,44.3458416518339));
#20948=CARTESIAN_POINT('Ctrl Pts',(177.666666666667,126.297687701072,44.3833333333333));
#20949=CARTESIAN_POINT('Ctrl Pts',(177.666666666667,126.2,44.3833333333333));
#20950=CARTESIAN_POINT('Ctrl Pts',(176.747537170301,126.999429809249,43.6801990080023));
#20951=CARTESIAN_POINT('Ctrl Pts',(176.943449124647,126.991962625601,43.8778707063143));
#20952=CARTESIAN_POINT('Ctrl Pts',(177.275869322433,126.85217227369,44.1891364044717));
#20953=CARTESIAN_POINT('Ctrl Pts',(177.553928344618,126.497803729337,44.4167983054418));
#20954=CARTESIAN_POINT('Ctrl Pts',(177.6,126.297687701072,44.45));
#20955=CARTESIAN_POINT('Ctrl Pts',(177.6,126.2,44.45));
#20956=CARTESIAN_POINT('Ctrl Pts',(176.747537170301,126.999429809249,43.6801990080023));
#20957=CARTESIAN_POINT('Ctrl Pts',(176.943449124647,126.991962625601,43.8778707063143));
#20958=CARTESIAN_POINT('Ctrl Pts',(177.275869322433,126.85217227369,44.1891364044717));
#20959=CARTESIAN_POINT('Ctrl Pts',(177.553928344618,126.497803729337,44.4167983054418));
#20960=CARTESIAN_POINT('Ctrl Pts',(177.6,126.297687701072,44.45));
#20961=CARTESIAN_POINT('Ctrl Pts',(177.6,126.2,44.45));
#20962=CARTESIAN_POINT('Ctrl Pts',(177.8,126.2,44.25));
#20963=CARTESIAN_POINT('Ctrl Pts',(177.8,126.297687701072,44.25));
#20964=CARTESIAN_POINT('Ctrl Pts',(177.766798305442,126.497803729337,44.2039283446181));
#20965=CARTESIAN_POINT('Ctrl Pts',(177.539136404472,126.85217227369,43.9258693224329));
#20966=CARTESIAN_POINT('Ctrl Pts',(177.227870706314,126.991962625601,43.5934491246469));
#20967=CARTESIAN_POINT('Ctrl Pts',(177.030199008002,126.999429809249,43.3975371703006));
#20968=CARTESIAN_POINT('Origin',(177.,126.2,6.35000000000001));
#20969=CARTESIAN_POINT('',(177.8,126.2,-107.75));
#20970=CARTESIAN_POINT('',(177.8,126.2,6.35000000000001));
#20971=CARTESIAN_POINT('',(177.030199008002,126.999429809249,-106.897537170301));
#20972=CARTESIAN_POINT('Ctrl Pts',(177.030199008002,126.999429809249,-106.897537170301));
#20973=CARTESIAN_POINT('Ctrl Pts',(177.227870706314,126.991962625601,-107.093449124647));
#20974=CARTESIAN_POINT('Ctrl Pts',(177.539138426476,126.852173302019,-107.425873068733));
#20975=CARTESIAN_POINT('Ctrl Pts',(177.766802032304,126.49780856488,-107.703932070819));
#20976=CARTESIAN_POINT('Ctrl Pts',(177.8,126.297687701072,-107.75));
#20977=CARTESIAN_POINT('Ctrl Pts',(177.8,126.2,-107.75));
#20978=CARTESIAN_POINT('',(177.,127.,-106.867705939749));
#20979=CARTESIAN_POINT('Ctrl Pts',(177.,127.,-106.867705939749));
#20980=CARTESIAN_POINT('Ctrl Pts',(177.000168736525,127.,-106.867872698805));
#20981=CARTESIAN_POINT('Ctrl Pts',(177.000340729475,126.999999960859,-106.868042672762));
#20982=CARTESIAN_POINT('Ctrl Pts',(177.000571968418,126.999999795533,-106.868271119852));
#20983=CARTESIAN_POINT('Ctrl Pts',(177.000827169104,126.999999613074,-106.868523239385));
#20984=CARTESIAN_POINT('Ctrl Pts',(177.00115445911,126.99999928102,-106.868846507485));
#20985=CARTESIAN_POINT('Ctrl Pts',(177.001581551272,126.999998436683,-106.869268262893));
#20986=CARTESIAN_POINT('Ctrl Pts',(177.002058527665,126.999997493728,-106.869739279202));
#20987=CARTESIAN_POINT('Ctrl Pts',(177.002659504952,126.999995895344,-106.870332661821));
#20988=CARTESIAN_POINT('Ctrl Pts',(177.003370507335,126.999992899769,-106.871034596213));
#20989=CARTESIAN_POINT('Ctrl Pts',(177.004269736312,126.999989111163,-106.871922356591));
#20990=CARTESIAN_POINT('Ctrl Pts',(177.005343532233,126.999982983391,-106.872982343061));
#20991=CARTESIAN_POINT('Ctrl Pts',(177.006495471841,126.999973630094,-106.874119373637));
#20992=CARTESIAN_POINT('Ctrl Pts',(177.007658170838,126.999964189434,-106.875267024348));
#20993=CARTESIAN_POINT('Ctrl Pts',(177.008895009794,126.999951463521,-106.876487764087));
#20994=CARTESIAN_POINT('Ctrl Pts',(177.010105362763,126.999936173481,-106.877682323415));
#20995=CARTESIAN_POINT('Ctrl Pts',(177.011011735643,126.999924723534,-106.878576869225));
#20996=CARTESIAN_POINT('Ctrl Pts',(177.011902720356,126.999911911841,-106.879456205747));
#20997=CARTESIAN_POINT('Ctrl Pts',(177.012763689538,126.999898173663,-106.880305951649));
#20998=CARTESIAN_POINT('Ctrl Pts',(177.013545386333,126.999885700406,-106.88107745853));
#20999=CARTESIAN_POINT('Ctrl Pts',(177.014301945281,126.999872502733,-106.881824182398));
#21000=CARTESIAN_POINT('Ctrl Pts',(177.01505431964,126.999858342121,-106.882566882091));
#21001=CARTESIAN_POINT('Ctrl Pts',(177.01584139004,126.999843528486,-106.883343831674));
#21002=CARTESIAN_POINT('Ctrl Pts',(177.016631142467,126.99982752742,-106.88412355571));
#21003=CARTESIAN_POINT('Ctrl Pts',(177.017448577774,126.999809694323,-106.88493080553));
#21004=CARTESIAN_POINT('Ctrl Pts',(177.018361167524,126.999789785346,-106.885832024142));
#21005=CARTESIAN_POINT('Ctrl Pts',(177.019307696952,126.999767552882,-106.88676699424));
#21006=CARTESIAN_POINT('Ctrl Pts',(177.020269575134,126.999743173978,-106.887717360133));
#21007=CARTESIAN_POINT('Ctrl Pts',(177.021527028359,126.999711303693,-106.888959763465));
#21008=CARTESIAN_POINT('Ctrl Pts',(177.02280899112,126.999675666215,-106.890226781854));
#21009=CARTESIAN_POINT('Ctrl Pts',(177.024000600934,126.999639900927,-106.891404811913));
#21010=CARTESIAN_POINT('Ctrl Pts',(177.024974456459,126.999610671373,-106.892367569242));
#21011=CARTESIAN_POINT('Ctrl Pts',(177.025884701841,126.999581516184,-106.893267661283));
#21012=CARTESIAN_POINT('Ctrl Pts',(177.026670911014,126.999555290462,-106.894045268365));
#21013=CARTESIAN_POINT('Ctrl Pts',(177.027355513698,126.999532454046,-106.894722380656));
#21014=CARTESIAN_POINT('Ctrl Pts',(177.027945163427,126.999511912239,-106.895305724143));
#21015=CARTESIAN_POINT('Ctrl Pts',(177.028424413854,126.999494873465,-106.895779966782));
#21016=CARTESIAN_POINT('Ctrl Pts',(177.028867379516,126.999479124722,-106.896218303804));
#21017=CARTESIAN_POINT('Ctrl Pts',(177.029215532932,126.999466401456,-106.896562942416));
#21018=CARTESIAN_POINT('Ctrl Pts',(177.02948815114,126.999456345864,-106.896832907358));
#21019=CARTESIAN_POINT('Ctrl Pts',(177.029741435771,126.999447003396,-106.897083726888));
#21020=CARTESIAN_POINT('Ctrl Pts',(177.029929301386,126.999439970325,-106.897269873308));
#21021=CARTESIAN_POINT('Ctrl Pts',(177.030100163957,126.999433537031,-106.897439207673));
#21022=CARTESIAN_POINT('Ctrl Pts',(177.030133469423,126.999432283018,-106.897472215253));
#21023=CARTESIAN_POINT('Ctrl Pts',(177.030166241246,126.999431047036,-106.897504695245));
#21024=CARTESIAN_POINT('Ctrl Pts',(177.030199008002,126.999429809249,-106.897537170301));
#21025=CARTESIAN_POINT('',(177.,127.,6.35000000000001));
#21026=CARTESIAN_POINT('Origin',(177.8,122.2375,44.45));
#21027=CARTESIAN_POINT('',(177.8,123.0375,-107.75));
#21028=CARTESIAN_POINT('',(177.8,123.0375,6.35000000000001));
#21029=CARTESIAN_POINT('',(177.8,122.2375,-107.75));
#21030=CARTESIAN_POINT('Origin',(177.,123.0375,6.35000000000001));
#21031=CARTESIAN_POINT('',(177.,122.2375,-106.867705939749));
#21032=CARTESIAN_POINT('',(177.,122.2375,6.35000000000001));
#21033=CARTESIAN_POINT('',(177.030199008002,122.238070190751,-106.897537170301));
#21034=CARTESIAN_POINT('Ctrl Pts',(177.030199008002,122.238070190751,-106.897537170301));
#21035=CARTESIAN_POINT('Ctrl Pts',(177.030030585505,122.238063828476,-106.897370247161));
#21036=CARTESIAN_POINT('Ctrl Pts',(177.029858909386,122.238057382362,-106.897200107149));
#21037=CARTESIAN_POINT('Ctrl Pts',(177.029628057339,122.23804882687,-106.896971463311));
#21038=CARTESIAN_POINT('Ctrl Pts',(177.029373282892,122.238039384803,-106.896719125902));
#21039=CARTESIAN_POINT('Ctrl Pts',(177.029046504163,122.238027372131,-106.896395602126));
#21040=CARTESIAN_POINT('Ctrl Pts',(177.028620026165,122.238012105093,-106.895973543409));
#21041=CARTESIAN_POINT('Ctrl Pts',(177.0281437326,122.237995054761,-106.895502185326));
#21042=CARTESIAN_POINT('Ctrl Pts',(177.027543563761,122.237973979824,-106.894908400156));
#21043=CARTESIAN_POINT('Ctrl Pts',(177.026833440411,122.237950147598,-106.894206022241));
#21044=CARTESIAN_POINT('Ctrl Pts',(177.025935290825,122.237920005083,-106.893317668924));
#21045=CARTESIAN_POINT('Ctrl Pts',(177.0248626695,122.237885609635,-106.892257012151));
#21046=CARTESIAN_POINT('Ctrl Pts',(177.023711822739,122.237851483799,-106.891119331008));
#21047=CARTESIAN_POINT('Ctrl Pts',(177.02255032393,122.2378170421,-106.889971119675));
#21048=CARTESIAN_POINT('Ctrl Pts',(177.021314608223,122.237783080562,-106.888749855389));
#21049=CARTESIAN_POINT('Ctrl Pts',(177.02010513109,122.237752675088,-106.887554886453));
#21050=CARTESIAN_POINT('Ctrl Pts',(177.019199401769,122.237729905638,-106.886660021744));
#21051=CARTESIAN_POINT('Ctrl Pts',(177.018308923963,122.237709074602,-106.885780431506));
#21052=CARTESIAN_POINT('Ctrl Pts',(177.01744828861,122.237690299368,-106.884930519969));
#21053=CARTESIAN_POINT('Ctrl Pts',(177.016666887982,122.237673252684,-106.884158855865));
#21054=CARTESIAN_POINT('Ctrl Pts',(177.015910483884,122.237657876347,-106.883412048069));
#21055=CARTESIAN_POINT('Ctrl Pts',(177.015158111372,122.237643618104,-106.882669339888));
#21056=CARTESIAN_POINT('Ctrl Pts',(177.014371053406,122.237628702536,-106.881892391791));
#21057=CARTESIAN_POINT('Ctrl Pts',(177.013581145558,122.237614869895,-106.881112751603));
#21058=CARTESIAN_POINT('Ctrl Pts',(177.012763400083,122.237601821718,-106.880305665967));
#21059=CARTESIAN_POINT('Ctrl Pts',(177.011850452579,122.237587254471,-106.879404619322));
#21060=CARTESIAN_POINT('Ctrl Pts',(177.010903370157,122.237573726381,-106.878469920094));
#21061=CARTESIAN_POINT('Ctrl Pts',(177.009940788518,122.237561764432,-106.877519896452));
#21062=CARTESIAN_POINT('Ctrl Pts',(177.008682347608,122.237546125856,-106.876277873367));
#21063=CARTESIAN_POINT('Ctrl Pts',(177.007399134233,122.237533328235,-106.875011353485));
#21064=CARTESIAN_POINT('Ctrl Pts',(177.006206223395,122.237524073618,-106.873833867007));
#21065=CARTESIAN_POINT('Ctrl Pts',(177.005231427341,122.237516511138,-106.872871675083));
#21066=CARTESIAN_POINT('Ctrl Pts',(177.004320197307,122.237511277906,-106.871972161594));
#21067=CARTESIAN_POINT('Ctrl Pts',(177.003533069744,122.237507801652,-106.871195084158));
#21068=CARTESIAN_POINT('Ctrl Pts',(177.00284764934,122.237504774575,-106.870518415274));
#21069=CARTESIAN_POINT('Ctrl Pts',(177.002257239436,122.237503040519,-106.869935482439));
#21070=CARTESIAN_POINT('Ctrl Pts',(177.001777334963,122.237501974327,-106.869461595743));
#21071=CARTESIAN_POINT('Ctrl Pts',(177.001333761302,122.237500988851,-106.869023584289));
#21072=CARTESIAN_POINT('Ctrl Pts',(177.000985093099,122.237500559908,-106.868679225686));
#21073=CARTESIAN_POINT('Ctrl Pts',(177.000712044088,122.237500316879,-106.868409497869));
#21074=CARTESIAN_POINT('Ctrl Pts',(177.000458357708,122.237500091084,-106.868158897168));
#21075=CARTESIAN_POINT('Ctrl Pts',(177.00027016379,122.237500027304,-106.867972933222));
#21076=CARTESIAN_POINT('Ctrl Pts',(177.000098987774,122.237500006124,-106.86780376677));
#21077=CARTESIAN_POINT('Ctrl Pts',(177.000065634445,122.237500001997,-106.867770805001));
#21078=CARTESIAN_POINT('Ctrl Pts',(177.000032814728,122.2375,-106.867738369912));
#21079=CARTESIAN_POINT('Ctrl Pts',(177.,122.2375,-106.867705939749));
#21080=CARTESIAN_POINT('Ctrl Pts',(177.8,123.0375,-107.75));
#21081=CARTESIAN_POINT('Ctrl Pts',(177.8,122.939812298928,-107.75));
#21082=CARTESIAN_POINT('Ctrl Pts',(177.76680186335,122.739691653929,-107.703931901455));
#21083=CARTESIAN_POINT('Ctrl Pts',(177.539138333658,122.385326746311,-107.42587289798));
#21084=CARTESIAN_POINT('Ctrl Pts',(177.227870706314,122.245537374399,-107.093449124647));
#21085=CARTESIAN_POINT('Ctrl Pts',(177.030199008002,122.238070190751,-106.897537170301));
#21086=CARTESIAN_POINT('Origin',(139.7,122.2375,-31.75));
#21087=CARTESIAN_POINT('',(102.682294060251,122.2375,43.65));
#21088=CARTESIAN_POINT('',(120.65,122.2375,43.65));
#21089=CARTESIAN_POINT('',(102.4,122.2375,43.3677059397485));
#21090=CARTESIAN_POINT('',(102.541147030126,122.2375,43.5088529698743));
#21091=CARTESIAN_POINT('',(102.4,122.2375,-106.867705939749));
#21092=CARTESIAN_POINT('',(102.4,122.2375,-69.85));
#21093=CARTESIAN_POINT('',(102.682294060251,122.2375,-107.15));
#21094=CARTESIAN_POINT('',(102.541147030126,122.2375,-107.008852969874));
#21095=CARTESIAN_POINT('',(176.717705939749,122.2375,-107.15));
#21096=CARTESIAN_POINT('',(158.75,122.2375,-107.15));
#21097=CARTESIAN_POINT('',(176.858852969874,122.2375,-107.008852969874));
#21098=CARTESIAN_POINT('Ctrl Pts',(177.030199008002,126.999429809249,-106.897537170301));
#21099=CARTESIAN_POINT('Ctrl Pts',(177.028516554556,126.999493365079,-106.895869694655));
#21100=CARTESIAN_POINT('Ctrl Pts',(177.016175572427,126.999932103249,-106.883668236945));
#21101=CARTESIAN_POINT('Ctrl Pts',(177.002608645735,126.99999591837,-106.870285389319));
#21102=CARTESIAN_POINT('Ctrl Pts',(177.000421407138,127.,-106.868122408304));
#21103=CARTESIAN_POINT('Ctrl Pts',(177.,127.,-106.867705939749));
#21104=CARTESIAN_POINT('Ctrl Pts',(176.935978395435,126.999429809249,-106.991757782868));
#21105=CARTESIAN_POINT('Ctrl Pts',(176.934300934589,126.999493365079,-106.990085314622));
#21106=CARTESIAN_POINT('Ctrl Pts',(176.92201328382,126.999932103249,-106.977830525551));
#21107=CARTESIAN_POINT('Ctrl Pts',(176.908498481157,126.99999591837,-106.964395553897));
#21108=CARTESIAN_POINT('Ctrl Pts',(176.90632174086,127.,-106.962222074582));
#21109=CARTESIAN_POINT('Ctrl Pts',(176.905901979916,127.,-106.961803959832));
#21110=CARTESIAN_POINT('Ctrl Pts',(176.841757782868,126.999429809249,-107.085978395435));
#21111=CARTESIAN_POINT('Ctrl Pts',(176.840085314622,126.999493365079,-107.084300934589));
#21112=CARTESIAN_POINT('Ctrl Pts',(176.827830525552,127.000007709825,-107.071972508603));
#21113=CARTESIAN_POINT('Ctrl Pts',(176.814395553897,126.999950502472,-107.058492828924));
#21114=CARTESIAN_POINT('Ctrl Pts',(176.812222074582,127.,-107.05632174086));
#21115=CARTESIAN_POINT('Ctrl Pts',(176.811803959832,127.,-107.055901979916));
#21116=CARTESIAN_POINT('Ctrl Pts',(176.747537170301,126.999429809249,-107.180199008002));
#21117=CARTESIAN_POINT('Ctrl Pts',(176.745869694655,126.999493365079,-107.178516554556));
#21118=CARTESIAN_POINT('Ctrl Pts',(176.733668236945,126.999932103249,-107.166175572427));
#21119=CARTESIAN_POINT('Ctrl Pts',(176.720285389319,126.99999591837,-107.152608645735));
#21120=CARTESIAN_POINT('Ctrl Pts',(176.718122408304,127.,-107.150421407138));
#21121=CARTESIAN_POINT('Ctrl Pts',(176.717705939749,127.,-107.15));
#21122=CARTESIAN_POINT('',(176.747537170301,126.999429809249,-107.180199008002));
#21123=CARTESIAN_POINT('Ctrl Pts',(176.747537170301,126.999429809249,-107.180199008002));
#21124=CARTESIAN_POINT('Ctrl Pts',(176.841757782868,126.999429809249,-107.085978395435));
#21125=CARTESIAN_POINT('Ctrl Pts',(176.935978395435,126.999429809249,-106.991757782868));
#21126=CARTESIAN_POINT('Ctrl Pts',(177.030199008002,126.999429809249,-106.897537170301));
#21127=CARTESIAN_POINT('',(176.717705939749,127.,-107.15));
#21128=CARTESIAN_POINT('Ctrl Pts',(176.747537170301,126.999429809249,-107.180199008002));
#21129=CARTESIAN_POINT('Ctrl Pts',(176.747370247161,126.999436171524,-107.180030585505));
#21130=CARTESIAN_POINT('Ctrl Pts',(176.747200107149,126.999442617638,-107.179858909386));
#21131=CARTESIAN_POINT('Ctrl Pts',(176.746971463311,126.99945117313,-107.179628057339));
#21132=CARTESIAN_POINT('Ctrl Pts',(176.746719125902,126.999460615197,-107.179373282892));
#21133=CARTESIAN_POINT('Ctrl Pts',(176.746395602126,126.999472627869,-107.179046504163));
#21134=CARTESIAN_POINT('Ctrl Pts',(176.745973543409,126.999487894907,-107.178620026165));
#21135=CARTESIAN_POINT('Ctrl Pts',(176.745502185327,126.999504945239,-107.1781437326));
#21136=CARTESIAN_POINT('Ctrl Pts',(176.744908400156,126.999526020176,-107.177543563761));
#21137=CARTESIAN_POINT('Ctrl Pts',(176.744206022241,126.999549852402,-107.176833440411));
#21138=CARTESIAN_POINT('Ctrl Pts',(176.743317668923,126.999579994917,-107.175935290825));
#21139=CARTESIAN_POINT('Ctrl Pts',(176.742257012151,126.999614390365,-107.1748626695));
#21140=CARTESIAN_POINT('Ctrl Pts',(176.741119331007,126.999648516201,-107.173711822738));
#21141=CARTESIAN_POINT('Ctrl Pts',(176.739971119675,126.9996829579,-107.17255032393));
#21142=CARTESIAN_POINT('Ctrl Pts',(176.738749855389,126.999716919438,-107.171314608223));
#21143=CARTESIAN_POINT('Ctrl Pts',(176.737554886453,126.999747324912,-107.17010513109));
#21144=CARTESIAN_POINT('Ctrl Pts',(176.736660021744,126.999770094362,-107.169199401769));
#21145=CARTESIAN_POINT('Ctrl Pts',(176.735780431506,126.999790925398,-107.168308923963));
#21146=CARTESIAN_POINT('Ctrl Pts',(176.734930519969,126.999809700632,-107.167448288609));
#21147=CARTESIAN_POINT('Ctrl Pts',(176.734158855869,126.999826747316,-107.166666887985));
#21148=CARTESIAN_POINT('Ctrl Pts',(176.733412048076,126.999842123653,-107.165910483891));
#21149=CARTESIAN_POINT('Ctrl Pts',(176.732669339899,126.999856381896,-107.165158111383));
#21150=CARTESIAN_POINT('Ctrl Pts',(176.731892391803,126.999871297464,-107.164371053417));
#21151=CARTESIAN_POINT('Ctrl Pts',(176.731112751615,126.999885130105,-107.16358114557));
#21152=CARTESIAN_POINT('Ctrl Pts',(176.730305665979,126.999898178281,-107.162763400095));
#21153=CARTESIAN_POINT('Ctrl Pts',(176.729404619336,126.999912745528,-107.161850452592));
#21154=CARTESIAN_POINT('Ctrl Pts',(176.728469920108,126.999926273619,-107.160903370172));
#21155=CARTESIAN_POINT('Ctrl Pts',(176.727519896467,126.999938235568,-107.159940788534));
#21156=CARTESIAN_POINT('Ctrl Pts',(176.726277873387,126.999953874144,-107.158682347629));
#21157=CARTESIAN_POINT('Ctrl Pts',(176.72501135351,126.999966671765,-107.157399134258));
#21158=CARTESIAN_POINT('Ctrl Pts',(176.723833867035,126.999975926382,-107.156206223424));
#21159=CARTESIAN_POINT('Ctrl Pts',(176.722871675108,126.999983488862,-107.155231427366));
#21160=CARTESIAN_POINT('Ctrl Pts',(176.721972161615,126.999988722094,-107.154320197329));
#21161=CARTESIAN_POINT('Ctrl Pts',(176.721195084176,126.999992198348,-107.153533069762));
#21162=CARTESIAN_POINT('Ctrl Pts',(176.72051841529,126.999995225425,-107.152847649357));
#21163=CARTESIAN_POINT('Ctrl Pts',(176.719935482452,126.999996959481,-107.15225723945));
#21164=CARTESIAN_POINT('Ctrl Pts',(176.719461595755,126.999998025673,-107.151777334975));
#21165=CARTESIAN_POINT('Ctrl Pts',(176.719023584299,126.999999011149,-107.151333761312));
#21166=CARTESIAN_POINT('Ctrl Pts',(176.718679225694,126.999999440092,-107.150985093108));
#21167=CARTESIAN_POINT('Ctrl Pts',(176.718409497876,126.999999683121,-107.150712044095));
#21168=CARTESIAN_POINT('Ctrl Pts',(176.718158897173,126.999999908916,-107.150458357714));
#21169=CARTESIAN_POINT('Ctrl Pts',(176.717972933227,126.999999972695,-107.150270163795));
#21170=CARTESIAN_POINT('Ctrl Pts',(176.717803766775,126.999999993876,-107.150098987779));
#21171=CARTESIAN_POINT('Ctrl Pts',(176.717770805004,126.999999998003,-107.150065634448));
#21172=CARTESIAN_POINT('Ctrl Pts',(176.717738369913,127.,-107.150032814729));
#21173=CARTESIAN_POINT('Ctrl Pts',(176.717705939749,127.,-107.15));
#21174=CARTESIAN_POINT('',(176.858852969874,127.,-107.008852969874));
#21175=CARTESIAN_POINT('Ctrl Pts',(176.747537170301,122.238070190751,-107.180199008002));
#21176=CARTESIAN_POINT('Ctrl Pts',(176.745869694655,122.238006634921,-107.178516554556));
#21177=CARTESIAN_POINT('Ctrl Pts',(176.733668171844,122.237567895484,-107.16617550697));
#21178=CARTESIAN_POINT('Ctrl Pts',(176.720285372322,122.237504081409,-107.152608628619));
#21179=CARTESIAN_POINT('Ctrl Pts',(176.718122408304,122.2375,-107.150421407138));
#21180=CARTESIAN_POINT('Ctrl Pts',(176.717705939749,122.2375,-107.15));
#21181=CARTESIAN_POINT('Ctrl Pts',(176.841757782868,122.238070190751,-107.085978395435));
#21182=CARTESIAN_POINT('Ctrl Pts',(176.840085314622,122.238006634921,-107.084300934589));
#21183=CARTESIAN_POINT('Ctrl Pts',(176.82783046045,122.237567895484,-107.072013218364));
#21184=CARTESIAN_POINT('Ctrl Pts',(176.8143955369,122.237504081409,-107.058498464041));
#21185=CARTESIAN_POINT('Ctrl Pts',(176.812222074582,122.2375,-107.05632174086));
#21186=CARTESIAN_POINT('Ctrl Pts',(176.811803959832,122.2375,-107.055901979916));
#21187=CARTESIAN_POINT('Ctrl Pts',(176.935978395435,122.238070190751,-106.991757782868));
#21188=CARTESIAN_POINT('Ctrl Pts',(176.934300934589,122.238006634921,-106.990085314622));
#21189=CARTESIAN_POINT('Ctrl Pts',(176.921972442847,122.237492296595,-106.97783046045));
#21190=CARTESIAN_POINT('Ctrl Pts',(176.908492811756,122.237549499319,-106.9643955369));
#21191=CARTESIAN_POINT('Ctrl Pts',(176.90632174086,122.2375,-106.962222074582));
#21192=CARTESIAN_POINT('Ctrl Pts',(176.905901979916,122.2375,-106.961803959832));
#21193=CARTESIAN_POINT('Ctrl Pts',(177.030199008002,122.238070190751,-106.897537170301));
#21194=CARTESIAN_POINT('Ctrl Pts',(177.028516554556,122.238006634921,-106.895869694655));
#21195=CARTESIAN_POINT('Ctrl Pts',(177.01617550697,122.237567895484,-106.883668171843));
#21196=CARTESIAN_POINT('Ctrl Pts',(177.002608628619,122.237504081409,-106.870285372322));
#21197=CARTESIAN_POINT('Ctrl Pts',(177.000421407138,122.2375,-106.868122408304));
#21198=CARTESIAN_POINT('Ctrl Pts',(177.,122.2375,-106.867705939749));
#21199=CARTESIAN_POINT('',(176.747537170301,122.238070190751,-107.180199008002));
#21200=CARTESIAN_POINT('Ctrl Pts',(176.717705939749,122.2375,-107.15));
#21201=CARTESIAN_POINT('Ctrl Pts',(176.717872698805,122.2375,-107.150168736525));
#21202=CARTESIAN_POINT('Ctrl Pts',(176.718042672762,122.237500039141,-107.150340729475));
#21203=CARTESIAN_POINT('Ctrl Pts',(176.718271119852,122.237500204467,-107.150571968418));
#21204=CARTESIAN_POINT('Ctrl Pts',(176.718523239385,122.237500386926,-107.150827169104));
#21205=CARTESIAN_POINT('Ctrl Pts',(176.718846507485,122.23750071898,-107.15115445911));
#21206=CARTESIAN_POINT('Ctrl Pts',(176.719268262893,122.237501563317,-107.151581551272));
#21207=CARTESIAN_POINT('Ctrl Pts',(176.719739279202,122.237502506272,-107.152058527665));
#21208=CARTESIAN_POINT('Ctrl Pts',(176.720332661821,122.237504104656,-107.152659504951));
#21209=CARTESIAN_POINT('Ctrl Pts',(176.721034596213,122.237507100231,-107.153370507335));
#21210=CARTESIAN_POINT('Ctrl Pts',(176.721922356591,122.237510888837,-107.154269736312));
#21211=CARTESIAN_POINT('Ctrl Pts',(176.72298234306,122.237517016609,-107.155343532233));
#21212=CARTESIAN_POINT('Ctrl Pts',(176.724119373636,122.237526369906,-107.15649547184));
#21213=CARTESIAN_POINT('Ctrl Pts',(176.725267024347,122.237535810566,-107.157658170837));
#21214=CARTESIAN_POINT('Ctrl Pts',(176.726487764087,122.237548536479,-107.158895009794));
#21215=CARTESIAN_POINT('Ctrl Pts',(176.727682323414,122.237563826519,-107.160105362763));
#21216=CARTESIAN_POINT('Ctrl Pts',(176.728576869224,122.237575276466,-107.161011735642));
#21217=CARTESIAN_POINT('Ctrl Pts',(176.729456205746,122.237588088159,-107.161902720355));
#21218=CARTESIAN_POINT('Ctrl Pts',(176.730305951649,122.237601826337,-107.162763689537));
#21219=CARTESIAN_POINT('Ctrl Pts',(176.731077458528,122.237614299594,-107.16354538633));
#21220=CARTESIAN_POINT('Ctrl Pts',(176.731824182394,122.237627497267,-107.164301945277));
#21221=CARTESIAN_POINT('Ctrl Pts',(176.732566882086,122.237641657879,-107.165054319635));
#21222=CARTESIAN_POINT('Ctrl Pts',(176.733343831668,122.237656471514,-107.165841390034));
#21223=CARTESIAN_POINT('Ctrl Pts',(176.734123555703,122.23767247258,-107.166631142461));
#21224=CARTESIAN_POINT('Ctrl Pts',(176.734930805524,122.237690305676,-107.167448577767));
#21225=CARTESIAN_POINT('Ctrl Pts',(176.735832024135,122.237710214654,-107.168361167517));
#21226=CARTESIAN_POINT('Ctrl Pts',(176.736766994232,122.237732447118,-107.169307696944));
#21227=CARTESIAN_POINT('Ctrl Pts',(176.737717360126,122.237756826022,-107.170269575126));
#21228=CARTESIAN_POINT('Ctrl Pts',(176.738959763455,122.237788696307,-107.171527028349));
#21229=CARTESIAN_POINT('Ctrl Pts',(176.740226781842,122.237824333784,-107.172808991109));
#21230=CARTESIAN_POINT('Ctrl Pts',(176.741404811901,122.237860099072,-107.174000600922));
#21231=CARTESIAN_POINT('Ctrl Pts',(176.742367569231,122.237889328627,-107.174974456448));
#21232=CARTESIAN_POINT('Ctrl Pts',(176.743267661274,122.237918483816,-107.175884701832));
#21233=CARTESIAN_POINT('Ctrl Pts',(176.744045268357,122.237944709538,-107.176670911006));
#21234=CARTESIAN_POINT('Ctrl Pts',(176.74472238065,122.237967545954,-107.17735551369));
#21235=CARTESIAN_POINT('Ctrl Pts',(176.745305724137,122.237988087761,-107.177945163421));
#21236=CARTESIAN_POINT('Ctrl Pts',(176.745779966777,122.238005126535,-107.178424413848));
#21237=CARTESIAN_POINT('Ctrl Pts',(176.7462183038,122.238020875278,-107.178867379512));
#21238=CARTESIAN_POINT('Ctrl Pts',(176.746562942412,122.238033598544,-107.179215532928));
#21239=CARTESIAN_POINT('Ctrl Pts',(176.746832907355,122.238043654136,-107.179488151137));
#21240=CARTESIAN_POINT('Ctrl Pts',(176.747083726886,122.238052996604,-107.179741435769));
#21241=CARTESIAN_POINT('Ctrl Pts',(176.747269873306,122.238060029674,-107.179929301384));
#21242=CARTESIAN_POINT('Ctrl Pts',(176.747439207671,122.238066462969,-107.180100163954));
#21243=CARTESIAN_POINT('Ctrl Pts',(176.747472215252,122.238067716982,-107.180133469422));
#21244=CARTESIAN_POINT('Ctrl Pts',(176.747504695245,122.238068952964,-107.180166241245));
#21245=CARTESIAN_POINT('Ctrl Pts',(176.747537170301,122.238070190751,-107.180199008002));
#21246=CARTESIAN_POINT('Ctrl Pts',(177.030199008002,122.238070190751,-106.897537170301));
#21247=CARTESIAN_POINT('Ctrl Pts',(176.935978395435,122.238070190751,-106.991757782868));
#21248=CARTESIAN_POINT('Ctrl Pts',(176.841757782868,122.238070190751,-107.085978395435));
#21249=CARTESIAN_POINT('Ctrl Pts',(176.747537170301,122.238070190751,-107.180199008002));
#21250=CARTESIAN_POINT('Ctrl Pts',(177.030199008002,122.238070190751,-106.897537170301));
#21251=CARTESIAN_POINT('Ctrl Pts',(177.227870706314,122.245537374399,-107.093449124647));
#21252=CARTESIAN_POINT('Ctrl Pts',(177.539138333658,122.385326746311,-107.42587289798));
#21253=CARTESIAN_POINT('Ctrl Pts',(177.76680186335,122.739691653929,-107.703931901455));
#21254=CARTESIAN_POINT('Ctrl Pts',(177.8,122.939812298928,-107.75));
#21255=CARTESIAN_POINT('Ctrl Pts',(177.8,123.0375,-107.75));
#21256=CARTESIAN_POINT('Ctrl Pts',(176.935978395435,122.238070190751,-106.991757782868));
#21257=CARTESIAN_POINT('Ctrl Pts',(177.133063512425,122.245537374399,-107.188256318536));
#21258=CARTESIAN_POINT('Ctrl Pts',(177.451383188432,122.385326746311,-107.513628043206));
#21259=CARTESIAN_POINT('Ctrl Pts',(177.695845209385,122.739691653929,-107.77488855542));
#21260=CARTESIAN_POINT('Ctrl Pts',(177.733333333333,122.939812298928,-107.816666666667));
#21261=CARTESIAN_POINT('Ctrl Pts',(177.733333333333,123.0375,-107.816666666667));
#21262=CARTESIAN_POINT('Ctrl Pts',(176.841757782868,122.238070190751,-107.085978395435));
#21263=CARTESIAN_POINT('Ctrl Pts',(177.038256318536,122.245537374399,-107.283063512425));
#21264=CARTESIAN_POINT('Ctrl Pts',(177.363628043206,122.385326746311,-107.601383188432));
#21265=CARTESIAN_POINT('Ctrl Pts',(177.62488855542,122.739691653929,-107.845845209385));
#21266=CARTESIAN_POINT('Ctrl Pts',(177.666666666667,122.939812298928,-107.883333333333));
#21267=CARTESIAN_POINT('Ctrl Pts',(177.666666666667,123.0375,-107.883333333333));
#21268=CARTESIAN_POINT('Ctrl Pts',(176.747537170301,122.238070190751,-107.180199008002));
#21269=CARTESIAN_POINT('Ctrl Pts',(176.943449124647,122.245537374399,-107.377870706314));
#21270=CARTESIAN_POINT('Ctrl Pts',(177.27587289798,122.385326746311,-107.689138333658));
#21271=CARTESIAN_POINT('Ctrl Pts',(177.553931901455,122.739691653929,-107.91680186335));
#21272=CARTESIAN_POINT('Ctrl Pts',(177.6,122.939812298928,-107.95));
#21273=CARTESIAN_POINT('Ctrl Pts',(177.6,123.0375,-107.95));
#21274=CARTESIAN_POINT('',(177.6,123.0375,-107.95));
#21275=CARTESIAN_POINT('Ctrl Pts',(176.747537170301,122.238070190751,-107.180199008002));
#21276=CARTESIAN_POINT('Ctrl Pts',(176.943449124647,122.245537374399,-107.377870706314));
#21277=CARTESIAN_POINT('Ctrl Pts',(177.27587289798,122.385326746311,-107.689138333658));
#21278=CARTESIAN_POINT('Ctrl Pts',(177.553931901455,122.739691653929,-107.91680186335));
#21279=CARTESIAN_POINT('Ctrl Pts',(177.6,122.939812298928,-107.95));
#21280=CARTESIAN_POINT('Ctrl Pts',(177.6,123.0375,-107.95));
#21281=CARTESIAN_POINT('',(177.6,123.0375,-107.95));
#21282=CARTESIAN_POINT('Origin',(177.7,122.2375,-107.85));
#21283=CARTESIAN_POINT('',(177.6,126.2,-107.95));
#21284=CARTESIAN_POINT('',(177.6,126.2,-107.95));
#21285=CARTESIAN_POINT('',(177.6,122.2375,-107.95));
#21286=CARTESIAN_POINT('Ctrl Pts',(176.747537170301,126.999429809249,-107.180199008002));
#21287=CARTESIAN_POINT('Ctrl Pts',(176.943449124647,126.991962625601,-107.377870706314));
#21288=CARTESIAN_POINT('Ctrl Pts',(177.275873068733,126.852173302019,-107.689138426476));
#21289=CARTESIAN_POINT('Ctrl Pts',(177.553932070819,126.49780856488,-107.916802032304));
#21290=CARTESIAN_POINT('Ctrl Pts',(177.6,126.297687701072,-107.95));
#21291=CARTESIAN_POINT('Ctrl Pts',(177.6,126.2,-107.95));
#21292=CARTESIAN_POINT('Ctrl Pts',(176.841757782868,126.999429809249,-107.085978395435));
#21293=CARTESIAN_POINT('Ctrl Pts',(177.038256318536,126.991962625601,-107.283063512425));
#21294=CARTESIAN_POINT('Ctrl Pts',(177.363628187981,126.852173302019,-107.601383307228));
#21295=CARTESIAN_POINT('Ctrl Pts',(177.624888724647,126.49780856488,-107.845845378476));
#21296=CARTESIAN_POINT('Ctrl Pts',(177.666666666667,126.297687701072,-107.883333333333));
#21297=CARTESIAN_POINT('Ctrl Pts',(177.666666666667,126.2,-107.883333333333));
#21298=CARTESIAN_POINT('Ctrl Pts',(176.935978395435,126.999429809249,-106.991757782868));
#21299=CARTESIAN_POINT('Ctrl Pts',(177.133063512425,126.991962625601,-107.188256318536));
#21300=CARTESIAN_POINT('Ctrl Pts',(177.451383307228,126.852173302019,-107.513628187981));
#21301=CARTESIAN_POINT('Ctrl Pts',(177.695845378476,126.49780856488,-107.774888724647));
#21302=CARTESIAN_POINT('Ctrl Pts',(177.733333333333,126.297687701072,-107.816666666667));
#21303=CARTESIAN_POINT('Ctrl Pts',(177.733333333333,126.2,-107.816666666667));
#21304=CARTESIAN_POINT('Ctrl Pts',(177.030199008002,126.999429809249,-106.897537170301));
#21305=CARTESIAN_POINT('Ctrl Pts',(177.227870706314,126.991962625601,-107.093449124647));
#21306=CARTESIAN_POINT('Ctrl Pts',(177.539138426476,126.852173302019,-107.425873068733));
#21307=CARTESIAN_POINT('Ctrl Pts',(177.766802032304,126.49780856488,-107.703932070819));
#21308=CARTESIAN_POINT('Ctrl Pts',(177.8,126.297687701072,-107.75));
#21309=CARTESIAN_POINT('Ctrl Pts',(177.8,126.2,-107.75));
#21310=CARTESIAN_POINT('Ctrl Pts',(177.6,126.2,-107.95));
#21311=CARTESIAN_POINT('Ctrl Pts',(177.6,126.297687701072,-107.95));
#21312=CARTESIAN_POINT('Ctrl Pts',(177.553932070819,126.49780856488,-107.916802032304));
#21313=CARTESIAN_POINT('Ctrl Pts',(177.275873068733,126.852173302019,-107.689138426476));
#21314=CARTESIAN_POINT('Ctrl Pts',(176.943449124647,126.991962625601,-107.377870706314));
#21315=CARTESIAN_POINT('Ctrl Pts',(176.747537170301,126.999429809249,-107.180199008002));
#21316=CARTESIAN_POINT('Origin',(158.75,126.2,-107.15));
#21317=CARTESIAN_POINT('',(101.8,126.2,-107.95));
#21318=CARTESIAN_POINT('',(158.75,126.2,-107.95));
#21319=CARTESIAN_POINT('',(102.652462829699,126.999429809249,-107.180199008002));
#21320=CARTESIAN_POINT('Ctrl Pts',(102.652462829699,126.999429809249,-107.180199008002));
#21321=CARTESIAN_POINT('Ctrl Pts',(102.456550875353,126.991962625601,-107.377870706314));
#21322=CARTESIAN_POINT('Ctrl Pts',(102.124131493119,126.852172058915,-107.68913596838));
#21323=CARTESIAN_POINT('Ctrl Pts',(101.846072469497,126.49780266677,-107.916797488447));
#21324=CARTESIAN_POINT('Ctrl Pts',(101.8,126.297687701072,-107.95));
#21325=CARTESIAN_POINT('Ctrl Pts',(101.8,126.2,-107.95));
#21326=CARTESIAN_POINT('',(102.682294060251,127.,-107.15));
#21327=CARTESIAN_POINT('Ctrl Pts',(102.682294060251,127.,-107.15));
#21328=CARTESIAN_POINT('Ctrl Pts',(102.682127301195,127.,-107.150168736525));
#21329=CARTESIAN_POINT('Ctrl Pts',(102.681957327238,126.999999960859,-107.150340729475));
#21330=CARTESIAN_POINT('Ctrl Pts',(102.681728880148,126.999999795533,-107.150571968418));
#21331=CARTESIAN_POINT('Ctrl Pts',(102.681476760615,126.999999613074,-107.150827169104));
#21332=CARTESIAN_POINT('Ctrl Pts',(102.681153492515,126.99999928102,-107.15115445911));
#21333=CARTESIAN_POINT('Ctrl Pts',(102.680731737107,126.999998436683,-107.151581551272));
#21334=CARTESIAN_POINT('Ctrl Pts',(102.680260720798,126.999997493728,-107.152058527665));
#21335=CARTESIAN_POINT('Ctrl Pts',(102.679667338179,126.999995895344,-107.152659504951));
#21336=CARTESIAN_POINT('Ctrl Pts',(102.678965403787,126.999992899769,-107.153370507335));
#21337=CARTESIAN_POINT('Ctrl Pts',(102.678077643409,126.999989111163,-107.154269736312));
#21338=CARTESIAN_POINT('Ctrl Pts',(102.67701765694,126.999982983391,-107.155343532233));
#21339=CARTESIAN_POINT('Ctrl Pts',(102.675880626364,126.999973630094,-107.156495471841));
#21340=CARTESIAN_POINT('Ctrl Pts',(102.674732975653,126.999964189434,-107.157658170837));
#21341=CARTESIAN_POINT('Ctrl Pts',(102.673512235913,126.999951463521,-107.158895009794));
#21342=CARTESIAN_POINT('Ctrl Pts',(102.672317676586,126.999936173481,-107.160105362763));
#21343=CARTESIAN_POINT('Ctrl Pts',(102.671423130776,126.999924723534,-107.161011735643));
#21344=CARTESIAN_POINT('Ctrl Pts',(102.670543794253,126.999911911841,-107.161902720355));
#21345=CARTESIAN_POINT('Ctrl Pts',(102.669694048351,126.999898173663,-107.162763689538));
#21346=CARTESIAN_POINT('Ctrl Pts',(102.66892254147,126.999885700406,-107.163545386333));
#21347=CARTESIAN_POINT('Ctrl Pts',(102.668175817602,126.999872502733,-107.164301945281));
#21348=CARTESIAN_POINT('Ctrl Pts',(102.667433117909,126.999858342121,-107.16505431964));
#21349=CARTESIAN_POINT('Ctrl Pts',(102.666656168326,126.999843528486,-107.16584139004));
#21350=CARTESIAN_POINT('Ctrl Pts',(102.66587644429,126.99982752742,-107.166631142467));
#21351=CARTESIAN_POINT('Ctrl Pts',(102.66506919447,126.999809694323,-107.167448577774));
#21352=CARTESIAN_POINT('Ctrl Pts',(102.664167975858,126.999789785346,-107.168361167524));
#21353=CARTESIAN_POINT('Ctrl Pts',(102.66323300576,126.999767552882,-107.169307696952));
#21354=CARTESIAN_POINT('Ctrl Pts',(102.662282639866,126.999743173978,-107.170269575135));
#21355=CARTESIAN_POINT('Ctrl Pts',(102.661040236535,126.999711303693,-107.171527028359));
#21356=CARTESIAN_POINT('Ctrl Pts',(102.659773218146,126.999675666215,-107.172808991121));
#21357=CARTESIAN_POINT('Ctrl Pts',(102.658595188086,126.999639900927,-107.174000600935));
#21358=CARTESIAN_POINT('Ctrl Pts',(102.657632430757,126.999610671373,-107.174974456459));
#21359=CARTESIAN_POINT('Ctrl Pts',(102.656732338716,126.999581516184,-107.175884701842));
#21360=CARTESIAN_POINT('Ctrl Pts',(102.655954731635,126.999555290462,-107.176670911014));
#21361=CARTESIAN_POINT('Ctrl Pts',(102.655277619343,126.999532454046,-107.177355513698));
#21362=CARTESIAN_POINT('Ctrl Pts',(102.654694275857,126.999511912239,-107.177945163427));
#21363=CARTESIAN_POINT('Ctrl Pts',(102.654220033218,126.999494873465,-107.178424413854));
#21364=CARTESIAN_POINT('Ctrl Pts',(102.653781696196,126.999479124722,-107.178867379516));
#21365=CARTESIAN_POINT('Ctrl Pts',(102.653437057584,126.999466401456,-107.179215532932));
#21366=CARTESIAN_POINT('Ctrl Pts',(102.653167092642,126.999456345864,-107.17948815114));
#21367=CARTESIAN_POINT('Ctrl Pts',(102.652916273112,126.999447003396,-107.179741435771));
#21368=CARTESIAN_POINT('Ctrl Pts',(102.652730126692,126.999439970325,-107.179929301386));
#21369=CARTESIAN_POINT('Ctrl Pts',(102.652560792327,126.999433537031,-107.180100163956));
#21370=CARTESIAN_POINT('Ctrl Pts',(102.652527784747,126.999432283018,-107.180133469423));
#21371=CARTESIAN_POINT('Ctrl Pts',(102.652495304755,126.999431047036,-107.180166241246));
#21372=CARTESIAN_POINT('Ctrl Pts',(102.652462829699,126.999429809249,-107.180199008002));
#21373=CARTESIAN_POINT('',(158.75,127.,-107.15));
#21374=CARTESIAN_POINT('Origin',(177.8,122.2375,-107.95));
#21375=CARTESIAN_POINT('',(101.8,123.0375,-107.95));
#21376=CARTESIAN_POINT('',(158.75,123.0375,-107.95));
#21377=CARTESIAN_POINT('',(101.8,122.2375,-107.95));
#21378=CARTESIAN_POINT('Origin',(158.75,123.0375,-107.15));
#21379=CARTESIAN_POINT('',(102.652462829699,122.238070190751,-107.180199008002));
#21380=CARTESIAN_POINT('Ctrl Pts',(102.652462829699,122.238070190751,-107.180199008002));
#21381=CARTESIAN_POINT('Ctrl Pts',(102.652629752839,122.238063828476,-107.180030585505));
#21382=CARTESIAN_POINT('Ctrl Pts',(102.652799892851,122.238057382362,-107.179858909386));
#21383=CARTESIAN_POINT('Ctrl Pts',(102.653028536689,122.23804882687,-107.179628057339));
#21384=CARTESIAN_POINT('Ctrl Pts',(102.653280874098,122.238039384803,-107.179373282892));
#21385=CARTESIAN_POINT('Ctrl Pts',(102.653604397874,122.238027372131,-107.179046504163));
#21386=CARTESIAN_POINT('Ctrl Pts',(102.654026456591,122.238012105093,-107.178620026165));
#21387=CARTESIAN_POINT('Ctrl Pts',(102.654497814673,122.237995054761,-107.1781437326));
#21388=CARTESIAN_POINT('Ctrl Pts',(102.655091599844,122.237973979824,-107.177543563761));
#21389=CARTESIAN_POINT('Ctrl Pts',(102.655793977759,122.237950147598,-107.176833440411));
#21390=CARTESIAN_POINT('Ctrl Pts',(102.656682331076,122.237920005083,-107.175935290825));
#21391=CARTESIAN_POINT('Ctrl Pts',(102.657742987849,122.237885609635,-107.1748626695));
#21392=CARTESIAN_POINT('Ctrl Pts',(102.658880668992,122.237851483799,-107.173711822739));
#21393=CARTESIAN_POINT('Ctrl Pts',(102.660028880325,122.2378170421,-107.17255032393));
#21394=CARTESIAN_POINT('Ctrl Pts',(102.661250144611,122.237783080562,-107.171314608223));
#21395=CARTESIAN_POINT('Ctrl Pts',(102.662445113547,122.237752675088,-107.17010513109));
#21396=CARTESIAN_POINT('Ctrl Pts',(102.663339978256,122.237729905638,-107.169199401769));
#21397=CARTESIAN_POINT('Ctrl Pts',(102.664219568494,122.237709074602,-107.168308923963));
#21398=CARTESIAN_POINT('Ctrl Pts',(102.665069480031,122.237690299368,-107.167448288609));
#21399=CARTESIAN_POINT('Ctrl Pts',(102.665841144133,122.237673252684,-107.166666887983));
#21400=CARTESIAN_POINT('Ctrl Pts',(102.666587951927,122.237657876347,-107.165910483887));
#21401=CARTESIAN_POINT('Ctrl Pts',(102.667330660107,122.237643618104,-107.165158111378));
#21402=CARTESIAN_POINT('Ctrl Pts',(102.668107608203,122.237628702536,-107.164371053412));
#21403=CARTESIAN_POINT('Ctrl Pts',(102.668887248391,122.237614869895,-107.163581145565));
#21404=CARTESIAN_POINT('Ctrl Pts',(102.669694334027,122.237601821718,-107.162763400089));
#21405=CARTESIAN_POINT('Ctrl Pts',(102.670595380671,122.237587254472,-107.161850452586));
#21406=CARTESIAN_POINT('Ctrl Pts',(102.671530079899,122.237573726381,-107.160903370165));
#21407=CARTESIAN_POINT('Ctrl Pts',(102.67248010354,122.237561764432,-107.159940788526));
#21408=CARTESIAN_POINT('Ctrl Pts',(102.673722126622,122.237546125856,-107.158682347619));
#21409=CARTESIAN_POINT('Ctrl Pts',(102.674988646501,122.237533328235,-107.157399134247));
#21410=CARTESIAN_POINT('Ctrl Pts',(102.676166132978,122.237524073618,-107.156206223411));
#21411=CARTESIAN_POINT('Ctrl Pts',(102.677128324903,122.237516511138,-107.155231427355));
#21412=CARTESIAN_POINT('Ctrl Pts',(102.678027838394,122.237511277906,-107.154320197319));
#21413=CARTESIAN_POINT('Ctrl Pts',(102.678804915832,122.237507801652,-107.153533069754));
#21414=CARTESIAN_POINT('Ctrl Pts',(102.679481584717,122.237504774575,-107.152847649349));
#21415=CARTESIAN_POINT('Ctrl Pts',(102.680064517554,122.237503040519,-107.152257239444));
#21416=CARTESIAN_POINT('Ctrl Pts',(102.68053840425,122.237501974327,-107.151777334969));
#21417=CARTESIAN_POINT('Ctrl Pts',(102.680976415705,122.237500988851,-107.151333761308));
#21418=CARTESIAN_POINT('Ctrl Pts',(102.681320774309,122.237500559908,-107.150985093104));
#21419=CARTESIAN_POINT('Ctrl Pts',(102.681590502127,122.237500316879,-107.150712044092));
#21420=CARTESIAN_POINT('Ctrl Pts',(102.681841102829,122.237500091084,-107.150458357711));
#21421=CARTESIAN_POINT('Ctrl Pts',(102.682027066775,122.237500027304,-107.150270163793));
#21422=CARTESIAN_POINT('Ctrl Pts',(102.682196233227,122.237500006124,-107.150098987777));
#21423=CARTESIAN_POINT('Ctrl Pts',(102.682229194998,122.237500001997,-107.150065634446));
#21424=CARTESIAN_POINT('Ctrl Pts',(102.682261630087,122.2375,-107.150032814729));
#21425=CARTESIAN_POINT('Ctrl Pts',(102.682294060251,122.2375,-107.15));
#21426=CARTESIAN_POINT('Ctrl Pts',(101.8,123.0375,-107.95));
#21427=CARTESIAN_POINT('Ctrl Pts',(101.8,122.939812298928,-107.95));
#21428=CARTESIAN_POINT('Ctrl Pts',(101.84607276554,122.739697720169,-107.916797191109));
#21429=CARTESIAN_POINT('Ctrl Pts',(102.124131789418,122.385328018291,-107.689135810314));
#21430=CARTESIAN_POINT('Ctrl Pts',(102.456550875353,122.245537374399,-107.377870706314));
#21431=CARTESIAN_POINT('Ctrl Pts',(102.652462829699,122.238070190751,-107.180199008002));
#21432=CARTESIAN_POINT('Ctrl Pts',(102.369800991998,122.238070190751,-106.897537170301));
#21433=CARTESIAN_POINT('Ctrl Pts',(102.371483445444,122.238006634921,-106.895869694655));
#21434=CARTESIAN_POINT('Ctrl Pts',(102.38382574621,122.237567871227,-106.883666925463));
#21435=CARTESIAN_POINT('Ctrl Pts',(102.397391698643,122.237504077204,-106.870285047339));
#21436=CARTESIAN_POINT('Ctrl Pts',(102.399578592862,122.2375,-106.868122408304));
#21437=CARTESIAN_POINT('Ctrl Pts',(102.4,122.2375,-106.867705939749));
#21438=CARTESIAN_POINT('Ctrl Pts',(102.464021604565,122.238070190751,-106.991757782868));
#21439=CARTESIAN_POINT('Ctrl Pts',(102.465699065411,122.238006634921,-106.990085314622));
#21440=CARTESIAN_POINT('Ctrl Pts',(102.477988034816,122.237567871227,-106.977829214069));
#21441=CARTESIAN_POINT('Ctrl Pts',(102.491501863221,122.237504077204,-106.964395211916));
#21442=CARTESIAN_POINT('Ctrl Pts',(102.49367825914,122.2375,-106.962222074582));
#21443=CARTESIAN_POINT('Ctrl Pts',(102.494098020084,122.2375,-106.961803959832));
#21444=CARTESIAN_POINT('Ctrl Pts',(102.558242217132,122.238070190751,-107.085978395435));
#21445=CARTESIAN_POINT('Ctrl Pts',(102.559914685378,122.238006634921,-107.084300934589));
#21446=CARTESIAN_POINT('Ctrl Pts',(102.572170785931,122.237492419513,-107.071971183941));
#21447=CARTESIAN_POINT('Ctrl Pts',(102.585604788083,122.237549533561,-107.058492483501));
#21448=CARTESIAN_POINT('Ctrl Pts',(102.587777925418,122.2375,-107.05632174086));
#21449=CARTESIAN_POINT('Ctrl Pts',(102.588196040168,122.2375,-107.055901979916));
#21450=CARTESIAN_POINT('Ctrl Pts',(102.652462829699,122.238070190751,-107.180199008002));
#21451=CARTESIAN_POINT('Ctrl Pts',(102.654130305345,122.238006634921,-107.178516554556));
#21452=CARTESIAN_POINT('Ctrl Pts',(102.666333074537,122.237567871227,-107.16617425379));
#21453=CARTESIAN_POINT('Ctrl Pts',(102.679714952661,122.237504077204,-107.152608301357));
#21454=CARTESIAN_POINT('Ctrl Pts',(102.681877591696,122.2375,-107.150421407138));
#21455=CARTESIAN_POINT('Ctrl Pts',(102.682294060251,122.2375,-107.15));
#21456=CARTESIAN_POINT('',(102.369800991998,122.238070190751,-106.897537170301));
#21457=CARTESIAN_POINT('Ctrl Pts',(102.4,122.2375,-106.867705939749));
#21458=CARTESIAN_POINT('Ctrl Pts',(102.399831263475,122.2375,-106.867872698805));
#21459=CARTESIAN_POINT('Ctrl Pts',(102.399659270525,122.237500039141,-106.868042672762));
#21460=CARTESIAN_POINT('Ctrl Pts',(102.399428031582,122.237500204467,-106.868271119852));
#21461=CARTESIAN_POINT('Ctrl Pts',(102.399172830896,122.237500386926,-106.868523239385));
#21462=CARTESIAN_POINT('Ctrl Pts',(102.39884554089,122.23750071898,-106.868846507485));
#21463=CARTESIAN_POINT('Ctrl Pts',(102.398418448728,122.237501563317,-106.869268262893));
#21464=CARTESIAN_POINT('Ctrl Pts',(102.397941472335,122.237502506272,-106.869739279202));
#21465=CARTESIAN_POINT('Ctrl Pts',(102.397340495049,122.237504104656,-106.870332661821));
#21466=CARTESIAN_POINT('Ctrl Pts',(102.396629492665,122.237507100231,-106.871034596213));
#21467=CARTESIAN_POINT('Ctrl Pts',(102.395730263688,122.237510888837,-106.871922356591));
#21468=CARTESIAN_POINT('Ctrl Pts',(102.394656467767,122.237517016609,-106.87298234306));
#21469=CARTESIAN_POINT('Ctrl Pts',(102.39350452816,122.237526369906,-106.874119373636));
#21470=CARTESIAN_POINT('Ctrl Pts',(102.392341829163,122.237535810566,-106.875267024347));
#21471=CARTESIAN_POINT('Ctrl Pts',(102.391104990206,122.237548536479,-106.876487764087));
#21472=CARTESIAN_POINT('Ctrl Pts',(102.389894637237,122.237563826519,-106.877682323414));
#21473=CARTESIAN_POINT('Ctrl Pts',(102.388988264358,122.237575276466,-106.878576869224));
#21474=CARTESIAN_POINT('Ctrl Pts',(102.388097279645,122.237588088159,-106.879456205746));
#21475=CARTESIAN_POINT('Ctrl Pts',(102.387236310463,122.237601826337,-106.880305951649));
#21476=CARTESIAN_POINT('Ctrl Pts',(102.386454613668,122.237614299594,-106.881077458529));
#21477=CARTESIAN_POINT('Ctrl Pts',(102.385698054719,122.237627497267,-106.881824182397));
#21478=CARTESIAN_POINT('Ctrl Pts',(102.38494568036,122.237641657879,-106.882566882091));
#21479=CARTESIAN_POINT('Ctrl Pts',(102.384158609961,122.237656471514,-106.883343831673));
#21480=CARTESIAN_POINT('Ctrl Pts',(102.383368857533,122.23767247258,-106.884123555709));
#21481=CARTESIAN_POINT('Ctrl Pts',(102.382551422227,122.237690305677,-106.88493080553));
#21482=CARTESIAN_POINT('Ctrl Pts',(102.381638832476,122.237710214654,-106.885832024142));
#21483=CARTESIAN_POINT('Ctrl Pts',(102.380692303048,122.237732447118,-106.886766994239));
#21484=CARTESIAN_POINT('Ctrl Pts',(102.379730424866,122.237756826022,-106.887717360133));
#21485=CARTESIAN_POINT('Ctrl Pts',(102.378472971641,122.237788696307,-106.888959763465));
#21486=CARTESIAN_POINT('Ctrl Pts',(102.377191008879,122.237824333785,-106.890226781854));
#21487=CARTESIAN_POINT('Ctrl Pts',(102.375999399065,122.237860099073,-106.891404811914));
#21488=CARTESIAN_POINT('Ctrl Pts',(102.375025543541,122.237889328627,-106.892367569243));
#21489=CARTESIAN_POINT('Ctrl Pts',(102.374115298158,122.237918483816,-106.893267661284));
#21490=CARTESIAN_POINT('Ctrl Pts',(102.373329088986,122.237944709538,-106.894045268365));
#21491=CARTESIAN_POINT('Ctrl Pts',(102.372644486302,122.237967545954,-106.894722380657));
#21492=CARTESIAN_POINT('Ctrl Pts',(102.372054836573,122.237988087761,-106.895305724143));
#21493=CARTESIAN_POINT('Ctrl Pts',(102.371575586146,122.238005126535,-106.895779966782));
#21494=CARTESIAN_POINT('Ctrl Pts',(102.371132620484,122.238020875278,-106.896218303804));
#21495=CARTESIAN_POINT('Ctrl Pts',(102.370784467068,122.238033598544,-106.896562942416));
#21496=CARTESIAN_POINT('Ctrl Pts',(102.37051184886,122.238043654136,-106.896832907358));
#21497=CARTESIAN_POINT('Ctrl Pts',(102.370258564229,122.238052996604,-106.897083726888));
#21498=CARTESIAN_POINT('Ctrl Pts',(102.370070698614,122.238060029675,-106.897269873308));
#21499=CARTESIAN_POINT('Ctrl Pts',(102.369899836044,122.238066462969,-106.897439207673));
#21500=CARTESIAN_POINT('Ctrl Pts',(102.369866530577,122.238067716982,-106.897472215253));
#21501=CARTESIAN_POINT('Ctrl Pts',(102.369833758754,122.238068952964,-106.897504695245));
#21502=CARTESIAN_POINT('Ctrl Pts',(102.369800991998,122.238070190751,-106.897537170301));
#21503=CARTESIAN_POINT('Ctrl Pts',(102.652462829699,122.238070190751,-107.180199008002));
#21504=CARTESIAN_POINT('Ctrl Pts',(102.558242217132,122.238070190751,-107.085978395435));
#21505=CARTESIAN_POINT('Ctrl Pts',(102.464021604565,122.238070190751,-106.991757782868));
#21506=CARTESIAN_POINT('Ctrl Pts',(102.369800991998,122.238070190751,-106.897537170301));
#21507=CARTESIAN_POINT('Ctrl Pts',(102.652462829699,126.999429809249,-107.180199008002));
#21508=CARTESIAN_POINT('Ctrl Pts',(102.654130305345,126.999493365079,-107.178516554556));
#21509=CARTESIAN_POINT('Ctrl Pts',(102.666332978446,126.999932126902,-107.166174350405));
#21510=CARTESIAN_POINT('Ctrl Pts',(102.679714927635,126.999995922473,-107.152608326559));
#21511=CARTESIAN_POINT('Ctrl Pts',(102.681877591696,127.,-107.150421407138));
#21512=CARTESIAN_POINT('Ctrl Pts',(102.682294060251,127.,-107.15));
#21513=CARTESIAN_POINT('Ctrl Pts',(102.558242217132,126.999429809249,-107.085978395435));
#21514=CARTESIAN_POINT('Ctrl Pts',(102.559914685378,126.999493365079,-107.084300934589));
#21515=CARTESIAN_POINT('Ctrl Pts',(102.572170689839,126.999932126902,-107.072012061799));
#21516=CARTESIAN_POINT('Ctrl Pts',(102.585604763057,126.999995922473,-107.058498161981));
#21517=CARTESIAN_POINT('Ctrl Pts',(102.587777925418,127.,-107.05632174086));
#21518=CARTESIAN_POINT('Ctrl Pts',(102.588196040168,127.,-107.055901979916));
#21519=CARTESIAN_POINT('Ctrl Pts',(102.464021604565,126.999429809249,-106.991757782868));
#21520=CARTESIAN_POINT('Ctrl Pts',(102.465699065411,126.999493365079,-106.990085314622));
#21521=CARTESIAN_POINT('Ctrl Pts',(102.478028719002,127.000007589963,-106.97782931016));
#21522=CARTESIAN_POINT('Ctrl Pts',(102.491507491221,126.999950469076,-106.964395236943));
#21523=CARTESIAN_POINT('Ctrl Pts',(102.49367825914,127.,-106.962222074582));
#21524=CARTESIAN_POINT('Ctrl Pts',(102.494098020084,127.,-106.961803959832));
#21525=CARTESIAN_POINT('Ctrl Pts',(102.369800991998,126.999429809249,-106.897537170301));
#21526=CARTESIAN_POINT('Ctrl Pts',(102.371483445444,126.999493365079,-106.895869694655));
#21527=CARTESIAN_POINT('Ctrl Pts',(102.383825649594,126.999932126902,-106.883667021554));
#21528=CARTESIAN_POINT('Ctrl Pts',(102.397391673441,126.999995922473,-106.870285072365));
#21529=CARTESIAN_POINT('Ctrl Pts',(102.399578592862,127.,-106.868122408304));
#21530=CARTESIAN_POINT('Ctrl Pts',(102.4,127.,-106.867705939749));
#21531=CARTESIAN_POINT('',(102.369800991998,126.999429809249,-106.897537170301));
#21532=CARTESIAN_POINT('Ctrl Pts',(102.369800991998,126.999429809249,-106.897537170301));
#21533=CARTESIAN_POINT('Ctrl Pts',(102.464021604565,126.999429809249,-106.991757782868));
#21534=CARTESIAN_POINT('Ctrl Pts',(102.558242217132,126.999429809249,-107.085978395435));
#21535=CARTESIAN_POINT('Ctrl Pts',(102.652462829699,126.999429809249,-107.180199008002));
#21536=CARTESIAN_POINT('',(102.4,127.,-106.867705939749));
#21537=CARTESIAN_POINT('Ctrl Pts',(102.369800991998,126.999429809249,-106.897537170301));
#21538=CARTESIAN_POINT('Ctrl Pts',(102.369969414495,126.999436171524,-106.897370247161));
#21539=CARTESIAN_POINT('Ctrl Pts',(102.370141090614,126.999442617638,-106.897200107149));
#21540=CARTESIAN_POINT('Ctrl Pts',(102.370371942661,126.99945117313,-106.896971463311));
#21541=CARTESIAN_POINT('Ctrl Pts',(102.370626717108,126.999460615197,-106.896719125902));
#21542=CARTESIAN_POINT('Ctrl Pts',(102.370953495837,126.999472627869,-106.896395602126));
#21543=CARTESIAN_POINT('Ctrl Pts',(102.371379973835,126.999487894907,-106.895973543409));
#21544=CARTESIAN_POINT('Ctrl Pts',(102.3718562674,126.999504945239,-106.895502185326));
#21545=CARTESIAN_POINT('Ctrl Pts',(102.372456436239,126.999526020176,-106.894908400156));
#21546=CARTESIAN_POINT('Ctrl Pts',(102.373166559589,126.999549852402,-106.894206022241));
#21547=CARTESIAN_POINT('Ctrl Pts',(102.374064709175,126.999579994917,-106.893317668923));
#21548=CARTESIAN_POINT('Ctrl Pts',(102.3751373305,126.999614390365,-106.892257012151));
#21549=CARTESIAN_POINT('Ctrl Pts',(102.376288177261,126.999648516201,-106.891119331007));
#21550=CARTESIAN_POINT('Ctrl Pts',(102.37744967607,126.9996829579,-106.889971119675));
#21551=CARTESIAN_POINT('Ctrl Pts',(102.378685391777,126.999716919438,-106.888749855389));
#21552=CARTESIAN_POINT('Ctrl Pts',(102.37989486891,126.999747324912,-106.887554886453));
#21553=CARTESIAN_POINT('Ctrl Pts',(102.380800598231,126.999770094362,-106.886660021744));
#21554=CARTESIAN_POINT('Ctrl Pts',(102.381691076037,126.999790925398,-106.885780431506));
#21555=CARTESIAN_POINT('Ctrl Pts',(102.382551711391,126.999809700632,-106.884930519969));
#21556=CARTESIAN_POINT('Ctrl Pts',(102.383333112013,126.999826747316,-106.884158855871));
#21557=CARTESIAN_POINT('Ctrl Pts',(102.384089516105,126.999842123653,-106.88341204808));
#21558=CARTESIAN_POINT('Ctrl Pts',(102.384841888611,126.999856381896,-106.882669339904));
#21559=CARTESIAN_POINT('Ctrl Pts',(102.385628946577,126.999871297464,-106.881892391808));
#21560=CARTESIAN_POINT('Ctrl Pts',(102.386418854424,126.999885130105,-106.881112751621));
#21561=CARTESIAN_POINT('Ctrl Pts',(102.387236599899,126.999898178281,-106.880305665985));
#21562=CARTESIAN_POINT('Ctrl Pts',(102.388149547401,126.999912745528,-106.879404619342));
#21563=CARTESIAN_POINT('Ctrl Pts',(102.389096629821,126.999926273619,-106.878469920115));
#21564=CARTESIAN_POINT('Ctrl Pts',(102.390059211459,126.999938235568,-106.877519896475));
#21565=CARTESIAN_POINT('Ctrl Pts',(102.391317652362,126.999953874144,-106.876277873397));
#21566=CARTESIAN_POINT('Ctrl Pts',(102.39260086573,126.999966671765,-106.875011353521));
#21567=CARTESIAN_POINT('Ctrl Pts',(102.393793776563,126.999975926382,-106.873833867047));
#21568=CARTESIAN_POINT('Ctrl Pts',(102.394768572622,126.999983488862,-106.87287167512));
#21569=CARTESIAN_POINT('Ctrl Pts',(102.395679802661,126.999988722094,-106.871972161625));
#21570=CARTESIAN_POINT('Ctrl Pts',(102.396466930229,126.999992198348,-106.871195084184));
#21571=CARTESIAN_POINT('Ctrl Pts',(102.397152350636,126.999995225425,-106.870518415297));
#21572=CARTESIAN_POINT('Ctrl Pts',(102.397742760543,126.999996959481,-106.869935482459));
#21573=CARTESIAN_POINT('Ctrl Pts',(102.39822266502,126.999998025673,-106.86946159576));
#21574=CARTESIAN_POINT('Ctrl Pts',(102.398666238683,126.999999011149,-106.869023584303));
#21575=CARTESIAN_POINT('Ctrl Pts',(102.399014906889,126.999999440092,-106.868679225698));
#21576=CARTESIAN_POINT('Ctrl Pts',(102.399287955902,126.999999683121,-106.868409497879));
#21577=CARTESIAN_POINT('Ctrl Pts',(102.399541642284,126.999999908916,-106.868158897176));
#21578=CARTESIAN_POINT('Ctrl Pts',(102.399729836203,126.999999972695,-106.867972933229));
#21579=CARTESIAN_POINT('Ctrl Pts',(102.399901012219,126.999999993876,-106.867803766777));
#21580=CARTESIAN_POINT('Ctrl Pts',(102.399934365551,126.999999998003,-106.867770805005));
#21581=CARTESIAN_POINT('Ctrl Pts',(102.39996718527,127.,-106.867738369914));
#21582=CARTESIAN_POINT('Ctrl Pts',(102.4,127.,-106.867705939749));
#21583=CARTESIAN_POINT('',(102.541147030126,127.,-107.008852969874));
#21584=CARTESIAN_POINT('Ctrl Pts',(102.369800991998,126.999429809249,-106.897537170301));
#21585=CARTESIAN_POINT('Ctrl Pts',(102.172129293686,126.991962625601,-107.093449124647));
#21586=CARTESIAN_POINT('Ctrl Pts',(101.86086403162,126.852172058915,-107.425868506881));
#21587=CARTESIAN_POINT('Ctrl Pts',(101.633202511553,126.49780266677,-107.703927530503));
#21588=CARTESIAN_POINT('Ctrl Pts',(101.6,126.297687701072,-107.75));
#21589=CARTESIAN_POINT('Ctrl Pts',(101.6,126.2,-107.75));
#21590=CARTESIAN_POINT('Ctrl Pts',(102.464021604565,126.999429809249,-106.991757782868));
#21591=CARTESIAN_POINT('Ctrl Pts',(102.266936487575,126.991962625601,-107.188256318536));
#21592=CARTESIAN_POINT('Ctrl Pts',(101.94861985212,126.852172058915,-107.513624327381));
#21593=CARTESIAN_POINT('Ctrl Pts',(101.704159164201,126.49780266677,-107.774884183151));
#21594=CARTESIAN_POINT('Ctrl Pts',(101.666666666667,126.297687701072,-107.816666666667));
#21595=CARTESIAN_POINT('Ctrl Pts',(101.666666666667,126.2,-107.816666666667));
#21596=CARTESIAN_POINT('Ctrl Pts',(102.558242217132,126.999429809249,-107.085978395435));
#21597=CARTESIAN_POINT('Ctrl Pts',(102.361743681464,126.991962625601,-107.283063512425));
#21598=CARTESIAN_POINT('Ctrl Pts',(102.03637567262,126.852172058915,-107.60138014788));
#21599=CARTESIAN_POINT('Ctrl Pts',(101.775115816849,126.49780266677,-107.845840835799));
#21600=CARTESIAN_POINT('Ctrl Pts',(101.733333333333,126.297687701072,-107.883333333333));
#21601=CARTESIAN_POINT('Ctrl Pts',(101.733333333333,126.2,-107.883333333333));
#21602=CARTESIAN_POINT('Ctrl Pts',(102.652462829699,126.999429809249,-107.180199008002));
#21603=CARTESIAN_POINT('Ctrl Pts',(102.456550875353,126.991962625601,-107.377870706314));
#21604=CARTESIAN_POINT('Ctrl Pts',(102.124131493119,126.852172058915,-107.68913596838));
#21605=CARTESIAN_POINT('Ctrl Pts',(101.846072469497,126.49780266677,-107.916797488447));
#21606=CARTESIAN_POINT('Ctrl Pts',(101.8,126.297687701072,-107.95));
#21607=CARTESIAN_POINT('Ctrl Pts',(101.8,126.2,-107.95));
#21608=CARTESIAN_POINT('',(101.6,126.2,-107.75));
#21609=CARTESIAN_POINT('',(101.8,126.2,-107.95));
#21610=CARTESIAN_POINT('Ctrl Pts',(101.6,126.2,-107.75));
#21611=CARTESIAN_POINT('Ctrl Pts',(101.6,126.297687701072,-107.75));
#21612=CARTESIAN_POINT('Ctrl Pts',(101.633202511553,126.49780266677,-107.703927530503));
#21613=CARTESIAN_POINT('Ctrl Pts',(101.86086403162,126.852172058915,-107.425868506881));
#21614=CARTESIAN_POINT('Ctrl Pts',(102.172129293686,126.991962625601,-107.093449124647));
#21615=CARTESIAN_POINT('Ctrl Pts',(102.369800991998,126.999429809249,-106.897537170301));
#21616=CARTESIAN_POINT('Origin',(101.7,122.2375,-107.85));
#21617=CARTESIAN_POINT('',(101.6,123.0375,-107.75));
#21618=CARTESIAN_POINT('',(101.8,123.0375,-107.95));
#21619=CARTESIAN_POINT('',(101.6,122.2375,-107.75));
#21620=CARTESIAN_POINT('Ctrl Pts',(102.652462829699,122.238070190751,-107.180199008002));
#21621=CARTESIAN_POINT('Ctrl Pts',(102.456550875353,122.245537374399,-107.377870706314));
#21622=CARTESIAN_POINT('Ctrl Pts',(102.124131789418,122.385328018291,-107.689135810314));
#21623=CARTESIAN_POINT('Ctrl Pts',(101.84607276554,122.739697720169,-107.916797191109));
#21624=CARTESIAN_POINT('Ctrl Pts',(101.8,122.939812298928,-107.95));
#21625=CARTESIAN_POINT('Ctrl Pts',(101.8,123.0375,-107.95));
#21626=CARTESIAN_POINT('Ctrl Pts',(102.558242217132,122.238070190751,-107.085978395435));
#21627=CARTESIAN_POINT('Ctrl Pts',(102.361743681464,122.245537374399,-107.283063512425));
#21628=CARTESIAN_POINT('Ctrl Pts',(102.036375922841,122.385328018291,-107.601379943736));
#21629=CARTESIAN_POINT('Ctrl Pts',(101.775116113324,122.739697720169,-107.845840538893));
#21630=CARTESIAN_POINT('Ctrl Pts',(101.733333333333,122.939812298928,-107.883333333333));
#21631=CARTESIAN_POINT('Ctrl Pts',(101.733333333333,123.0375,-107.883333333333));
#21632=CARTESIAN_POINT('Ctrl Pts',(102.464021604565,122.238070190751,-106.991757782868));
#21633=CARTESIAN_POINT('Ctrl Pts',(102.266936487575,122.245537374399,-107.188256318536));
#21634=CARTESIAN_POINT('Ctrl Pts',(101.948620056264,122.385328018291,-107.513624077159));
#21635=CARTESIAN_POINT('Ctrl Pts',(101.704159461107,122.739697720169,-107.774883886676));
#21636=CARTESIAN_POINT('Ctrl Pts',(101.666666666667,122.939812298928,-107.816666666667));
#21637=CARTESIAN_POINT('Ctrl Pts',(101.666666666667,123.0375,-107.816666666667));
#21638=CARTESIAN_POINT('Ctrl Pts',(102.369800991998,122.238070190751,-106.897537170301));
#21639=CARTESIAN_POINT('Ctrl Pts',(102.172129293686,122.245537374399,-107.093449124647));
#21640=CARTESIAN_POINT('Ctrl Pts',(101.860864189686,122.385328018291,-107.425868210582));
#21641=CARTESIAN_POINT('Ctrl Pts',(101.633202808891,122.739697720169,-107.70392723446));
#21642=CARTESIAN_POINT('Ctrl Pts',(101.6,122.939812298928,-107.75));
#21643=CARTESIAN_POINT('Ctrl Pts',(101.6,123.0375,-107.75));
#21644=CARTESIAN_POINT('Ctrl Pts',(102.369800991998,122.238070190751,-106.897537170301));
#21645=CARTESIAN_POINT('Ctrl Pts',(102.172129293686,122.245537374399,-107.093449124647));
#21646=CARTESIAN_POINT('Ctrl Pts',(101.860864189686,122.385328018291,-107.425868210582));
#21647=CARTESIAN_POINT('Ctrl Pts',(101.633202808891,122.739697720169,-107.70392723446));
#21648=CARTESIAN_POINT('Ctrl Pts',(101.6,122.939812298928,-107.75));
#21649=CARTESIAN_POINT('Ctrl Pts',(101.6,123.0375,-107.75));
#21650=CARTESIAN_POINT('Ctrl Pts',(102.652462829699,122.238070190751,43.6801990080023));
#21651=CARTESIAN_POINT('Ctrl Pts',(102.654130305345,122.238006634921,43.678516554556));
#21652=CARTESIAN_POINT('Ctrl Pts',(102.666334669584,122.237567840162,43.6661726500475));
#21653=CARTESIAN_POINT('Ctrl Pts',(102.679715367383,122.237504071867,43.6526078837211));
#21654=CARTESIAN_POINT('Ctrl Pts',(102.681877591696,122.2375,43.6504214071384));
#21655=CARTESIAN_POINT('Ctrl Pts',(102.682294060251,122.2375,43.65));
#21656=CARTESIAN_POINT('Ctrl Pts',(102.558242217132,122.238070190751,43.5859783954351));
#21657=CARTESIAN_POINT('Ctrl Pts',(102.559914685378,122.238006634921,43.584300934589));
#21658=CARTESIAN_POINT('Ctrl Pts',(102.572172380978,122.237567840162,43.5720103614411));
#21659=CARTESIAN_POINT('Ctrl Pts',(102.585605202805,122.237504071867,43.5584977191432));
#21660=CARTESIAN_POINT('Ctrl Pts',(102.587777925418,122.2375,43.5563217408604));
#21661=CARTESIAN_POINT('Ctrl Pts',(102.588196040168,122.2375,43.5559019799162));
#21662=CARTESIAN_POINT('Ctrl Pts',(102.464021604565,122.238070190751,43.4917577828678));
#21663=CARTESIAN_POINT('Ctrl Pts',(102.465699065411,122.238006634921,43.490085314622));
#21664=CARTESIAN_POINT('Ctrl Pts',(102.478030427135,122.237492576792,43.4778276190222));
#21665=CARTESIAN_POINT('Ctrl Pts',(102.491507935396,122.237549577289,43.4643947971951));
#21666=CARTESIAN_POINT('Ctrl Pts',(102.49367825914,122.2375,43.4622220745823));
#21667=CARTESIAN_POINT('Ctrl Pts',(102.494098020084,122.2375,43.4618039598323));
#21668=CARTESIAN_POINT('Ctrl Pts',(102.369800991998,122.238070190751,43.3975371703006));
#21669=CARTESIAN_POINT('Ctrl Pts',(102.371483445444,122.238006634921,43.3958696946549));
#21670=CARTESIAN_POINT('Ctrl Pts',(102.383827349952,122.237567840162,43.3836653304159));
#21671=CARTESIAN_POINT('Ctrl Pts',(102.397392116279,122.237504071867,43.3702846326172));
#21672=CARTESIAN_POINT('Ctrl Pts',(102.399578592862,122.2375,43.3681224083043));
#21673=CARTESIAN_POINT('Ctrl Pts',(102.4,122.2375,43.3677059397485));
#21674=CARTESIAN_POINT('',(102.652462829699,122.238070190751,43.6801990080023));
#21675=CARTESIAN_POINT('Ctrl Pts',(102.682294060251,122.2375,43.65));
#21676=CARTESIAN_POINT('Ctrl Pts',(102.682127301195,122.2375,43.650168736525));
#21677=CARTESIAN_POINT('Ctrl Pts',(102.681957327238,122.237500039141,43.6503407294752));
#21678=CARTESIAN_POINT('Ctrl Pts',(102.681728880148,122.237500204467,43.6505719684178));
#21679=CARTESIAN_POINT('Ctrl Pts',(102.681476760615,122.237500386926,43.6508271691041));
#21680=CARTESIAN_POINT('Ctrl Pts',(102.681153492515,122.23750071898,43.6511544591101));
#21681=CARTESIAN_POINT('Ctrl Pts',(102.680731737107,122.237501563317,43.6515815512717));
#21682=CARTESIAN_POINT('Ctrl Pts',(102.680260720798,122.237502506272,43.6520585276647));
#21683=CARTESIAN_POINT('Ctrl Pts',(102.679667338179,122.237504104656,43.6526595049514));
#21684=CARTESIAN_POINT('Ctrl Pts',(102.678965403787,122.237507100231,43.6533705073352));
#21685=CARTESIAN_POINT('Ctrl Pts',(102.678077643409,122.237510888837,43.654269736312));
#21686=CARTESIAN_POINT('Ctrl Pts',(102.67701765694,122.237517016609,43.6553435322326));
#21687=CARTESIAN_POINT('Ctrl Pts',(102.675880626364,122.237526369906,43.6564954718404));
#21688=CARTESIAN_POINT('Ctrl Pts',(102.674732975653,122.237535810566,43.657658170837));
#21689=CARTESIAN_POINT('Ctrl Pts',(102.673512235913,122.237548536479,43.6588950097936));
#21690=CARTESIAN_POINT('Ctrl Pts',(102.672317676586,122.237563826519,43.6601053627627));
#21691=CARTESIAN_POINT('Ctrl Pts',(102.671423130776,122.237575276466,43.6610117356424));
#21692=CARTESIAN_POINT('Ctrl Pts',(102.670543794254,122.237588088159,43.6619027203553));
#21693=CARTESIAN_POINT('Ctrl Pts',(102.669694048351,122.237601826337,43.6627636895375));
#21694=CARTESIAN_POINT('Ctrl Pts',(102.66892254147,122.237614299594,43.6635453863333));
#21695=CARTESIAN_POINT('Ctrl Pts',(102.668175817601,122.237627497267,43.6643019452827));
#21696=CARTESIAN_POINT('Ctrl Pts',(102.667433117906,122.237641657879,43.665054319643));
#21697=CARTESIAN_POINT('Ctrl Pts',(102.666656168324,122.237656471514,43.6658413900421));
#21698=CARTESIAN_POINT('Ctrl Pts',(102.665876444288,122.23767247258,43.6666311424699));
#21699=CARTESIAN_POINT('Ctrl Pts',(102.665069194467,122.237690305677,43.6674485777763));
#21700=CARTESIAN_POINT('Ctrl Pts',(102.664167975855,122.237710214654,43.6683611675272));
#21701=CARTESIAN_POINT('Ctrl Pts',(102.663233005757,122.237732447118,43.6693076969552));
#21702=CARTESIAN_POINT('Ctrl Pts',(102.662282639863,122.237756826022,43.6702695751378));
#21703=CARTESIAN_POINT('Ctrl Pts',(102.661040236531,122.237788696307,43.6715270283636));
#21704=CARTESIAN_POINT('Ctrl Pts',(102.659773218141,122.237824333785,43.6728089911263));
#21705=CARTESIAN_POINT('Ctrl Pts',(102.65859518808,122.237860099073,43.6740006009409));
#21706=CARTESIAN_POINT('Ctrl Pts',(102.657632430752,122.237889328627,43.6749744564645));
#21707=CARTESIAN_POINT('Ctrl Pts',(102.656732338711,122.237918483816,43.6758847018465));
#21708=CARTESIAN_POINT('Ctrl Pts',(102.655954731631,122.237944709538,43.6766709110183));
#21709=CARTESIAN_POINT('Ctrl Pts',(102.65527761934,122.237967545954,43.6773555137014));
#21710=CARTESIAN_POINT('Ctrl Pts',(102.654694275854,122.237988087761,43.6779451634301));
#21711=CARTESIAN_POINT('Ctrl Pts',(102.654220033215,122.238005126535,43.6784244138562));
#21712=CARTESIAN_POINT('Ctrl Pts',(102.653781696193,122.238020875278,43.6788673795183));
#21713=CARTESIAN_POINT('Ctrl Pts',(102.653437057583,122.238033598544,43.6792155329338));
#21714=CARTESIAN_POINT('Ctrl Pts',(102.65316709264,122.238043654136,43.6794881511416));
#21715=CARTESIAN_POINT('Ctrl Pts',(102.65291627311,122.238052996604,43.6797414357727));
#21716=CARTESIAN_POINT('Ctrl Pts',(102.652730126691,122.238060029675,43.679929301387));
#21717=CARTESIAN_POINT('Ctrl Pts',(102.652560792326,122.238066462969,43.6801001639574));
#21718=CARTESIAN_POINT('Ctrl Pts',(102.652527784746,122.238067716982,43.6801334694235));
#21719=CARTESIAN_POINT('Ctrl Pts',(102.652495304755,122.238068952964,43.6801662412459));
#21720=CARTESIAN_POINT('Ctrl Pts',(102.652462829699,122.238070190751,43.6801990080023));
#21721=CARTESIAN_POINT('',(102.369800991998,122.238070190751,43.3975371703006));
#21722=CARTESIAN_POINT('Ctrl Pts',(102.369800991998,122.238070190751,43.3975371703006));
#21723=CARTESIAN_POINT('Ctrl Pts',(102.464021604565,122.238070190751,43.4917577828678));
#21724=CARTESIAN_POINT('Ctrl Pts',(102.558242217132,122.238070190751,43.5859783954351));
#21725=CARTESIAN_POINT('Ctrl Pts',(102.652462829699,122.238070190751,43.6801990080023));
#21726=CARTESIAN_POINT('Ctrl Pts',(102.369800991998,122.238070190751,43.3975371703006));
#21727=CARTESIAN_POINT('Ctrl Pts',(102.369969414495,122.238063828476,43.3973702471606));
#21728=CARTESIAN_POINT('Ctrl Pts',(102.370141090614,122.238057382362,43.397200107149));
#21729=CARTESIAN_POINT('Ctrl Pts',(102.370371942661,122.23804882687,43.3969714633111));
#21730=CARTESIAN_POINT('Ctrl Pts',(102.370626717108,122.238039384803,43.3967191259023));
#21731=CARTESIAN_POINT('Ctrl Pts',(102.370953495837,122.238027372131,43.3963956021262));
#21732=CARTESIAN_POINT('Ctrl Pts',(102.371379973835,122.238012105093,43.3959735434091));
#21733=CARTESIAN_POINT('Ctrl Pts',(102.3718562674,122.237995054761,43.3955021853265));
#21734=CARTESIAN_POINT('Ctrl Pts',(102.372456436239,122.237973979824,43.3949084001559));
#21735=CARTESIAN_POINT('Ctrl Pts',(102.373166559589,122.237950147598,43.3942060222409));
#21736=CARTESIAN_POINT('Ctrl Pts',(102.374064709175,122.237920005083,43.3933176689235));
#21737=CARTESIAN_POINT('Ctrl Pts',(102.3751373305,122.237885609635,43.3922570121515));
#21738=CARTESIAN_POINT('Ctrl Pts',(102.376288177261,122.237851483799,43.391119331008));
#21739=CARTESIAN_POINT('Ctrl Pts',(102.37744967607,122.2378170421,43.3899711196755));
#21740=CARTESIAN_POINT('Ctrl Pts',(102.378685391777,122.237783080562,43.3887498553894));
#21741=CARTESIAN_POINT('Ctrl Pts',(102.37989486891,122.237752675088,43.3875548864534));
#21742=CARTESIAN_POINT('Ctrl Pts',(102.38080059823,122.237729905638,43.386660021744));
#21743=CARTESIAN_POINT('Ctrl Pts',(102.381691076037,122.237709074602,43.385780431506));
#21744=CARTESIAN_POINT('Ctrl Pts',(102.38255171139,122.237690299368,43.3849305199691));
#21745=CARTESIAN_POINT('Ctrl Pts',(102.383333112017,122.237673252684,43.3841588558664));
#21746=CARTESIAN_POINT('Ctrl Pts',(102.384089516114,122.237657876347,43.3834120480707));
#21747=CARTESIAN_POINT('Ctrl Pts',(102.384841888625,122.237643618104,43.3826693398905));
#21748=CARTESIAN_POINT('Ctrl Pts',(102.385628946591,122.237628702536,43.3818923917941));
#21749=CARTESIAN_POINT('Ctrl Pts',(102.386418854439,122.237614869895,43.3811127516064));
#21750=CARTESIAN_POINT('Ctrl Pts',(102.387236599914,122.237601821718,43.3803056659701));
#21751=CARTESIAN_POINT('Ctrl Pts',(102.388149547418,122.237587254471,43.3794046193259));
#21752=CARTESIAN_POINT('Ctrl Pts',(102.389096629839,122.237573726381,43.3784699200974));
#21753=CARTESIAN_POINT('Ctrl Pts',(102.390059211478,122.237561764432,43.3775198964558));
#21754=CARTESIAN_POINT('Ctrl Pts',(102.391317652386,122.237546125856,43.3762778733733));
#21755=CARTESIAN_POINT('Ctrl Pts',(102.392600865758,122.237533328235,43.3750113534931));
#21756=CARTESIAN_POINT('Ctrl Pts',(102.393793776595,122.237524073618,43.3738338670164));
#21757=CARTESIAN_POINT('Ctrl Pts',(102.394768572651,122.237516511138,43.372871675092));
#21758=CARTESIAN_POINT('Ctrl Pts',(102.395679802686,122.237511277906,43.371972161601));
#21759=CARTESIAN_POINT('Ctrl Pts',(102.39646693025,122.237507801652,43.3711950841639));
#21760=CARTESIAN_POINT('Ctrl Pts',(102.397152350654,122.237504774575,43.3705184152794));
#21761=CARTESIAN_POINT('Ctrl Pts',(102.397742760559,122.237503040519,43.3699354824433));
#21762=CARTESIAN_POINT('Ctrl Pts',(102.398222665033,122.237501974327,43.3694615957471));
#21763=CARTESIAN_POINT('Ctrl Pts',(102.398666238694,122.237500988851,43.3690235842925));
#21764=CARTESIAN_POINT('Ctrl Pts',(102.399014906898,122.237500559908,43.3686792256888));
#21765=CARTESIAN_POINT('Ctrl Pts',(102.399287955909,122.237500316879,43.368409497871));
#21766=CARTESIAN_POINT('Ctrl Pts',(102.39954164229,122.237500091084,43.3681588971694));
#21767=CARTESIAN_POINT('Ctrl Pts',(102.399729836208,122.237500027304,43.3679729332236));
#21768=CARTESIAN_POINT('Ctrl Pts',(102.399901012224,122.237500006124,43.3678037667716));
#21769=CARTESIAN_POINT('Ctrl Pts',(102.399934365554,122.237500001997,43.3677708050016));
#21770=CARTESIAN_POINT('Ctrl Pts',(102.399967185272,122.2375,43.3677383699122));
#21771=CARTESIAN_POINT('Ctrl Pts',(102.4,122.2375,43.3677059397485));
#21772=CARTESIAN_POINT('Ctrl Pts',(102.369800991998,126.999429809249,43.3975371703006));
#21773=CARTESIAN_POINT('Ctrl Pts',(102.371483445444,126.999493365079,43.395869694655));
#21774=CARTESIAN_POINT('Ctrl Pts',(102.383827204795,126.999932157025,43.3836654747861));
#21775=CARTESIAN_POINT('Ctrl Pts',(102.397392078533,126.999995927652,43.3702846700996));
#21776=CARTESIAN_POINT('Ctrl Pts',(102.399578592862,127.,43.3681224083043));
#21777=CARTESIAN_POINT('Ctrl Pts',(102.4,127.,43.3677059397485));
#21778=CARTESIAN_POINT('Ctrl Pts',(102.464021604565,126.999429809249,43.4917577828679));
#21779=CARTESIAN_POINT('Ctrl Pts',(102.465699065411,126.999493365079,43.490085314622));
#21780=CARTESIAN_POINT('Ctrl Pts',(102.477989493402,126.999932157025,43.4778277633925));
#21781=CARTESIAN_POINT('Ctrl Pts',(102.491502243111,126.999995927652,43.4643948346774));
#21782=CARTESIAN_POINT('Ctrl Pts',(102.49367825914,127.,43.4622220745824));
#21783=CARTESIAN_POINT('Ctrl Pts',(102.494098020084,127.,43.4618039598323));
#21784=CARTESIAN_POINT('Ctrl Pts',(102.558242217132,126.999429809249,43.5859783954351));
#21785=CARTESIAN_POINT('Ctrl Pts',(102.559914685378,126.999493365079,43.584300934589));
#21786=CARTESIAN_POINT('Ctrl Pts',(102.572172236607,127.000007437442,43.5719697186859));
#21787=CARTESIAN_POINT('Ctrl Pts',(102.585605165322,126.999950426665,43.558492102464));
#21788=CARTESIAN_POINT('Ctrl Pts',(102.587777925418,127.,43.5563217408604));
#21789=CARTESIAN_POINT('Ctrl Pts',(102.588196040168,127.,43.5559019799162));
#21790=CARTESIAN_POINT('Ctrl Pts',(102.652462829699,126.999429809249,43.6801990080024));
#21791=CARTESIAN_POINT('Ctrl Pts',(102.654130305345,126.999493365079,43.6785165545561));
#21792=CARTESIAN_POINT('Ctrl Pts',(102.666334525214,126.999932157025,43.6661727952046));
#21793=CARTESIAN_POINT('Ctrl Pts',(102.6797153299,126.999995927652,43.6526079214671));
#21794=CARTESIAN_POINT('Ctrl Pts',(102.681877591696,127.,43.6504214071384));
#21795=CARTESIAN_POINT('Ctrl Pts',(102.682294060251,127.,43.65));
#21796=CARTESIAN_POINT('',(102.4,127.,43.3677059397485));
#21797=CARTESIAN_POINT('',(102.369800991998,126.999429809249,43.3975371703006));
#21798=CARTESIAN_POINT('Ctrl Pts',(102.4,127.,43.3677059397485));
#21799=CARTESIAN_POINT('Ctrl Pts',(102.399831263475,127.,43.3678726988052));
#21800=CARTESIAN_POINT('Ctrl Pts',(102.399659270525,126.999999960859,43.3680426727623));
#21801=CARTESIAN_POINT('Ctrl Pts',(102.399428031582,126.999999795533,43.3682711198523));
#21802=CARTESIAN_POINT('Ctrl Pts',(102.399172830896,126.999999613074,43.368523239385));
#21803=CARTESIAN_POINT('Ctrl Pts',(102.39884554089,126.99999928102,43.3688465074853));
#21804=CARTESIAN_POINT('Ctrl Pts',(102.398418448728,126.999998436683,43.3692682628935));
#21805=CARTESIAN_POINT('Ctrl Pts',(102.397941472335,126.999997493728,43.3697392792018));
#21806=CARTESIAN_POINT('Ctrl Pts',(102.397340495048,126.999995895344,43.3703326618209));
#21807=CARTESIAN_POINT('Ctrl Pts',(102.396629492664,126.999992899769,43.3710345962131));
#21808=CARTESIAN_POINT('Ctrl Pts',(102.395730263688,126.999989111163,43.3719223565914));
#21809=CARTESIAN_POINT('Ctrl Pts',(102.394656467767,126.999982983391,43.3729823430605));
#21810=CARTESIAN_POINT('Ctrl Pts',(102.393504528159,126.999973630094,43.3741193736366));
#21811=CARTESIAN_POINT('Ctrl Pts',(102.392341829162,126.999964189434,43.3752670243476));
#21812=CARTESIAN_POINT('Ctrl Pts',(102.391104990206,126.999951463521,43.3764877640872));
#21813=CARTESIAN_POINT('Ctrl Pts',(102.389894637237,126.999936173481,43.3776823234144));
#21814=CARTESIAN_POINT('Ctrl Pts',(102.388988264357,126.999924723534,43.3785768692246));
#21815=CARTESIAN_POINT('Ctrl Pts',(102.388097279644,126.999911911841,43.379456205747));
#21816=CARTESIAN_POINT('Ctrl Pts',(102.387236310462,126.999898173663,43.3803059516493));
#21817=CARTESIAN_POINT('Ctrl Pts',(102.386454613667,126.999885700406,43.3810774585302));
#21818=CARTESIAN_POINT('Ctrl Pts',(102.385698054718,126.999872502733,43.3818241823982));
#21819=CARTESIAN_POINT('Ctrl Pts',(102.384945680359,126.999858342121,43.3825668820919));
#21820=CARTESIAN_POINT('Ctrl Pts',(102.38415860996,126.999843528486,43.3833438316742));
#21821=CARTESIAN_POINT('Ctrl Pts',(102.383368857532,126.99982752742,43.3841235557102));
#21822=CARTESIAN_POINT('Ctrl Pts',(102.382551422226,126.999809694323,43.3849308055307));
#21823=CARTESIAN_POINT('Ctrl Pts',(102.381638832475,126.999789785346,43.3858320241431));
#21824=CARTESIAN_POINT('Ctrl Pts',(102.380692303047,126.999767552882,43.3867669942407));
#21825=CARTESIAN_POINT('Ctrl Pts',(102.379730424864,126.999743173978,43.3877173601347));
#21826=CARTESIAN_POINT('Ctrl Pts',(102.378472971639,126.999711303693,43.3889597634663));
#21827=CARTESIAN_POINT('Ctrl Pts',(102.377191008877,126.999675666215,43.390226781856));
#21828=CARTESIAN_POINT('Ctrl Pts',(102.375999399063,126.999639900927,43.3914048119161));
#21829=CARTESIAN_POINT('Ctrl Pts',(102.375025543539,126.999610671373,43.3923675692448));
#21830=CARTESIAN_POINT('Ctrl Pts',(102.374115298156,126.999581516184,43.3932676612859));
#21831=CARTESIAN_POINT('Ctrl Pts',(102.373329088984,126.999555290462,43.3940452683668));
#21832=CARTESIAN_POINT('Ctrl Pts',(102.372644486301,126.999532454046,43.3947223806583));
#21833=CARTESIAN_POINT('Ctrl Pts',(102.372054836572,126.999511912239,43.3953057241444));
#21834=CARTESIAN_POINT('Ctrl Pts',(102.371575586145,126.999494873465,43.3957799667835));
#21835=CARTESIAN_POINT('Ctrl Pts',(102.371132620483,126.999479124722,43.3962183038054));
#21836=CARTESIAN_POINT('Ctrl Pts',(102.370784467067,126.999466401456,43.3965629424164));
#21837=CARTESIAN_POINT('Ctrl Pts',(102.370511848859,126.999456345864,43.3968329073587));
#21838=CARTESIAN_POINT('Ctrl Pts',(102.370258564228,126.999447003396,43.3970837268889));
#21839=CARTESIAN_POINT('Ctrl Pts',(102.370070698614,126.999439970325,43.3972698733084));
#21840=CARTESIAN_POINT('Ctrl Pts',(102.369899836043,126.999433537031,43.3974392076734));
#21841=CARTESIAN_POINT('Ctrl Pts',(102.369866530577,126.999432283018,43.3974722152535));
#21842=CARTESIAN_POINT('Ctrl Pts',(102.369833758754,126.999431047036,43.3975046952453));
#21843=CARTESIAN_POINT('Ctrl Pts',(102.369800991998,126.999429809249,43.3975371703006));
#21844=CARTESIAN_POINT('',(102.652462829699,126.999429809249,43.6801990080024));
#21845=CARTESIAN_POINT('Ctrl Pts',(102.652462829699,126.999429809249,43.6801990080024));
#21846=CARTESIAN_POINT('Ctrl Pts',(102.558242217132,126.999429809249,43.5859783954351));
#21847=CARTESIAN_POINT('Ctrl Pts',(102.464021604565,126.999429809249,43.4917577828679));
#21848=CARTESIAN_POINT('Ctrl Pts',(102.369800991998,126.999429809249,43.3975371703006));
#21849=CARTESIAN_POINT('',(102.682294060251,127.,43.65));
#21850=CARTESIAN_POINT('Ctrl Pts',(102.652462829699,126.999429809249,43.6801990080024));
#21851=CARTESIAN_POINT('Ctrl Pts',(102.652629752839,126.999436171524,43.6800305855052));
#21852=CARTESIAN_POINT('Ctrl Pts',(102.652799892851,126.999442617638,43.6798589093858));
#21853=CARTESIAN_POINT('Ctrl Pts',(102.653028536689,126.99945117313,43.6796280573389));
#21854=CARTESIAN_POINT('Ctrl Pts',(102.653280874098,126.999460615197,43.6793732828919));
#21855=CARTESIAN_POINT('Ctrl Pts',(102.653604397874,126.999472627869,43.6790465041629));
#21856=CARTESIAN_POINT('Ctrl Pts',(102.654026456591,126.999487894907,43.6786200261654));
#21857=CARTESIAN_POINT('Ctrl Pts',(102.654497814673,126.999504945239,43.6781437326003));
#21858=CARTESIAN_POINT('Ctrl Pts',(102.655091599844,126.999526020176,43.6775435637606));
#21859=CARTESIAN_POINT('Ctrl Pts',(102.655793977759,126.999549852402,43.6768334404111));
#21860=CARTESIAN_POINT('Ctrl Pts',(102.656682331077,126.999579994917,43.6759352908252));
#21861=CARTESIAN_POINT('Ctrl Pts',(102.657742987849,126.999614390365,43.6748626694998));
#21862=CARTESIAN_POINT('Ctrl Pts',(102.658880668993,126.999648516201,43.6737118227386));
#21863=CARTESIAN_POINT('Ctrl Pts',(102.660028880325,126.9996829579,43.6725503239297));
#21864=CARTESIAN_POINT('Ctrl Pts',(102.661250144611,126.999716919438,43.6713146082226));
#21865=CARTESIAN_POINT('Ctrl Pts',(102.662445113547,126.999747324912,43.67010513109));
#21866=CARTESIAN_POINT('Ctrl Pts',(102.663339978256,126.999770094362,43.6691994017692));
#21867=CARTESIAN_POINT('Ctrl Pts',(102.664219568494,126.999790925398,43.6683089239629));
#21868=CARTESIAN_POINT('Ctrl Pts',(102.665069480031,126.999809700632,43.6674482886094));
#21869=CARTESIAN_POINT('Ctrl Pts',(102.66584114413,126.999826747316,43.6666668879864));
#21870=CARTESIAN_POINT('Ctrl Pts',(102.666587951922,126.999842123653,43.6659104838931));
#21871=CARTESIAN_POINT('Ctrl Pts',(102.667330660098,126.999856381896,43.6651581113864));
#21872=CARTESIAN_POINT('Ctrl Pts',(102.668107608194,126.999871297464,43.6643710534204));
#21873=CARTESIAN_POINT('Ctrl Pts',(102.668887248382,126.999885130105,43.6635811455735));
#21874=CARTESIAN_POINT('Ctrl Pts',(102.669694334017,126.999898178281,43.6627634000984));
#21875=CARTESIAN_POINT('Ctrl Pts',(102.670595380661,126.999912745528,43.6618504525959));
#21876=CARTESIAN_POINT('Ctrl Pts',(102.671530079888,126.999926273619,43.6609033701756));
#21877=CARTESIAN_POINT('Ctrl Pts',(102.672480103529,126.999938235568,43.6599407885377));
#21878=CARTESIAN_POINT('Ctrl Pts',(102.673722126608,126.999953874144,43.6586823476335));
#21879=CARTESIAN_POINT('Ctrl Pts',(102.674988646484,126.999966671765,43.6573991342643));
#21880=CARTESIAN_POINT('Ctrl Pts',(102.676166132959,126.999975926382,43.6562062234303));
#21881=CARTESIAN_POINT('Ctrl Pts',(102.677128324886,126.999983488862,43.6552314273719));
#21882=CARTESIAN_POINT('Ctrl Pts',(102.67802783838,126.999988722094,43.6543201973338));
#21883=CARTESIAN_POINT('Ctrl Pts',(102.67880491582,126.999992198348,43.6535330697665));
#21884=CARTESIAN_POINT('Ctrl Pts',(102.679481584706,126.999995225425,43.6528476493604));
#21885=CARTESIAN_POINT('Ctrl Pts',(102.680064517544,126.999996959481,43.6522572394536));
#21886=CARTESIAN_POINT('Ctrl Pts',(102.680538404243,126.999998025673,43.6517773349774));
#21887=CARTESIAN_POINT('Ctrl Pts',(102.680976415699,126.999999011149,43.6513337613144));
#21888=CARTESIAN_POINT('Ctrl Pts',(102.681320774304,126.999999440092,43.6509850931095));
#21889=CARTESIAN_POINT('Ctrl Pts',(102.681590502123,126.999999683121,43.6507120440968));
#21890=CARTESIAN_POINT('Ctrl Pts',(102.681841102826,126.999999908916,43.650458357715));
#21891=CARTESIAN_POINT('Ctrl Pts',(102.682027066772,126.999999972695,43.6502701637959));
#21892=CARTESIAN_POINT('Ctrl Pts',(102.682196233224,126.999999993876,43.6500989877796));
#21893=CARTESIAN_POINT('Ctrl Pts',(102.682229194996,126.999999998003,43.6500656344483));
#21894=CARTESIAN_POINT('Ctrl Pts',(102.682261630086,127.,43.6500328147295));
#21895=CARTESIAN_POINT('Ctrl Pts',(102.682294060251,127.,43.65));
#21896=CARTESIAN_POINT('',(102.541147030126,127.,43.5088529698743));
#21897=CARTESIAN_POINT('Ctrl Pts',(102.652462829699,126.999429809249,43.6801990080024));
#21898=CARTESIAN_POINT('Ctrl Pts',(102.456550875353,126.991962625601,43.8778707063143));
#21899=CARTESIAN_POINT('Ctrl Pts',(102.124136995242,126.852170699062,44.1891330663933));
#21900=CARTESIAN_POINT('Ctrl Pts',(101.846077990743,126.497795401137,44.4167919209351));
#21901=CARTESIAN_POINT('Ctrl Pts',(101.8,126.297687701072,44.45));
#21902=CARTESIAN_POINT('Ctrl Pts',(101.8,126.2,44.45));
#21903=CARTESIAN_POINT('Ctrl Pts',(102.558242217132,126.999429809249,43.5859783954351));
#21904=CARTESIAN_POINT('Ctrl Pts',(102.361743681464,126.991962625601,43.7830635124252));
#21905=CARTESIAN_POINT('Ctrl Pts',(102.03638030803,126.852170699062,44.1013763791816));
#21906=CARTESIAN_POINT('Ctrl Pts',(101.775121353517,126.497795401137,44.3458352837092));
#21907=CARTESIAN_POINT('Ctrl Pts',(101.733333333333,126.297687701072,44.3833333333333));
#21908=CARTESIAN_POINT('Ctrl Pts',(101.733333333333,126.2,44.3833333333333));
#21909=CARTESIAN_POINT('Ctrl Pts',(102.464021604565,126.999429809249,43.4917577828679));
#21910=CARTESIAN_POINT('Ctrl Pts',(102.266936487575,126.991962625601,43.6882563185361));
#21911=CARTESIAN_POINT('Ctrl Pts',(101.948623620818,126.852170699062,44.0136196919698));
#21912=CARTESIAN_POINT('Ctrl Pts',(101.704164716291,126.497795401137,44.2748786464833));
#21913=CARTESIAN_POINT('Ctrl Pts',(101.666666666667,126.297687701072,44.3166666666667));
#21914=CARTESIAN_POINT('Ctrl Pts',(101.666666666667,126.2,44.3166666666667));
#21915=CARTESIAN_POINT('Ctrl Pts',(102.369800991998,126.999429809249,43.3975371703006));
#21916=CARTESIAN_POINT('Ctrl Pts',(102.172129293686,126.991962625601,43.5934491246469));
#21917=CARTESIAN_POINT('Ctrl Pts',(101.860866933607,126.852170699062,43.9258630047581));
#21918=CARTESIAN_POINT('Ctrl Pts',(101.633208079065,126.497795401137,44.2039220092575));
#21919=CARTESIAN_POINT('Ctrl Pts',(101.6,126.297687701072,44.25));
#21920=CARTESIAN_POINT('Ctrl Pts',(101.6,126.2,44.25));
#21921=CARTESIAN_POINT('',(101.6,126.2,44.25));
#21922=CARTESIAN_POINT('Ctrl Pts',(102.369800991998,126.999429809249,43.3975371703006));
#21923=CARTESIAN_POINT('Ctrl Pts',(102.172129293686,126.991962625601,43.5934491246469));
#21924=CARTESIAN_POINT('Ctrl Pts',(101.860866933607,126.852170699062,43.9258630047581));
#21925=CARTESIAN_POINT('Ctrl Pts',(101.633208079065,126.497795401137,44.2039220092575));
#21926=CARTESIAN_POINT('Ctrl Pts',(101.6,126.297687701072,44.25));
#21927=CARTESIAN_POINT('Ctrl Pts',(101.6,126.2,44.25));
#21928=CARTESIAN_POINT('',(101.8,126.2,44.45));
#21929=CARTESIAN_POINT('',(101.6,126.2,44.25));
#21930=CARTESIAN_POINT('Ctrl Pts',(101.8,126.2,44.45));
#21931=CARTESIAN_POINT('Ctrl Pts',(101.8,126.297687701072,44.45));
#21932=CARTESIAN_POINT('Ctrl Pts',(101.846077990743,126.497795401137,44.4167919209351));
#21933=CARTESIAN_POINT('Ctrl Pts',(102.124136995242,126.852170699062,44.1891330663933));
#21934=CARTESIAN_POINT('Ctrl Pts',(102.456550875353,126.991962625601,43.8778707063143));
#21935=CARTESIAN_POINT('Ctrl Pts',(102.652462829699,126.999429809249,43.6801990080024));
#21936=CARTESIAN_POINT('Origin',(101.7,122.2375,44.35));
#21937=CARTESIAN_POINT('',(101.6,123.0375,44.25));
#21938=CARTESIAN_POINT('',(101.6,122.2375,44.25));
#21939=CARTESIAN_POINT('',(101.8,123.0375,44.45));
#21940=CARTESIAN_POINT('',(101.6,123.0375,44.25));
#21941=CARTESIAN_POINT('',(101.8,122.2375,44.45));
#21942=CARTESIAN_POINT('Ctrl Pts',(101.8,123.0375,44.45));
#21943=CARTESIAN_POINT('Ctrl Pts',(101.8,122.939812298928,44.45));
#21944=CARTESIAN_POINT('Ctrl Pts',(101.846078418479,122.739705166155,44.4167914876269));
#21945=CARTESIAN_POINT('Ctrl Pts',(102.124137419351,122.385329399097,44.1891328457024));
#21946=CARTESIAN_POINT('Ctrl Pts',(102.456550875353,122.245537374399,43.8778707063143));
#21947=CARTESIAN_POINT('Ctrl Pts',(102.652462829699,122.238070190751,43.6801990080023));
#21948=CARTESIAN_POINT('Ctrl Pts',(101.733333333333,123.0375,44.3833333333333));
#21949=CARTESIAN_POINT('Ctrl Pts',(101.733333333333,122.939812298928,44.3833333333333));
#21950=CARTESIAN_POINT('Ctrl Pts',(101.77512178311,122.739705166155,44.3458348522582));
#21951=CARTESIAN_POINT('Ctrl Pts',(102.036380664333,122.385329399097,44.1013760906846));
#21952=CARTESIAN_POINT('Ctrl Pts',(102.361743681464,122.245537374399,43.7830635124252));
#21953=CARTESIAN_POINT('Ctrl Pts',(102.558242217132,122.238070190751,43.5859783954351));
#21954=CARTESIAN_POINT('Ctrl Pts',(101.666666666667,123.0375,44.3166666666667));
#21955=CARTESIAN_POINT('Ctrl Pts',(101.666666666667,122.939812298928,44.3166666666667));
#21956=CARTESIAN_POINT('Ctrl Pts',(101.704165147742,122.739705166155,44.2748782168895));
#21957=CARTESIAN_POINT('Ctrl Pts',(101.948623909315,122.385329399097,44.0136193356668));
#21958=CARTESIAN_POINT('Ctrl Pts',(102.266936487575,122.245537374399,43.688256318536));
#21959=CARTESIAN_POINT('Ctrl Pts',(102.464021604565,122.238070190751,43.4917577828678));
#21960=CARTESIAN_POINT('Ctrl Pts',(101.6,123.0375,44.25));
#21961=CARTESIAN_POINT('Ctrl Pts',(101.6,122.939812298928,44.25));
#21962=CARTESIAN_POINT('Ctrl Pts',(101.633208512373,122.739705166155,44.2039215815208));
#21963=CARTESIAN_POINT('Ctrl Pts',(101.860867154298,122.385329399097,43.925862580649));
#21964=CARTESIAN_POINT('Ctrl Pts',(102.172129293686,122.245537374399,43.5934491246469));
#21965=CARTESIAN_POINT('Ctrl Pts',(102.369800991998,122.238070190751,43.3975371703006));
#21966=CARTESIAN_POINT('Ctrl Pts',(102.652462829699,122.238070190751,43.6801990080023));
#21967=CARTESIAN_POINT('Ctrl Pts',(102.456550875353,122.245537374399,43.8778707063143));
#21968=CARTESIAN_POINT('Ctrl Pts',(102.124137419351,122.385329399097,44.1891328457024));
#21969=CARTESIAN_POINT('Ctrl Pts',(101.846078418479,122.739705166155,44.4167914876269));
#21970=CARTESIAN_POINT('Ctrl Pts',(101.8,122.939812298928,44.45));
#21971=CARTESIAN_POINT('Ctrl Pts',(101.8,123.0375,44.45));
#21972=CARTESIAN_POINT('Ctrl Pts',(101.6,123.0375,44.25));
#21973=CARTESIAN_POINT('Ctrl Pts',(101.6,122.939812298928,44.25));
#21974=CARTESIAN_POINT('Ctrl Pts',(101.633208512373,122.739705166155,44.2039215815208));
#21975=CARTESIAN_POINT('Ctrl Pts',(101.860867154298,122.385329399097,43.925862580649));
#21976=CARTESIAN_POINT('Ctrl Pts',(102.172129293686,122.245537374399,43.5934491246469));
#21977=CARTESIAN_POINT('Ctrl Pts',(102.369800991998,122.238070190751,43.3975371703006));
#21978=CARTESIAN_POINT('Origin',(102.4,123.0375,-69.85));
#21979=CARTESIAN_POINT('',(101.6,123.0375,-69.85));
#21980=CARTESIAN_POINT('Origin',(101.6,122.2375,-107.95));
#21981=CARTESIAN_POINT('',(101.6,126.2,-69.85));
#21982=CARTESIAN_POINT('Origin',(102.4,126.2,-69.85));
#21983=CARTESIAN_POINT('',(102.4,127.,-69.85));
#21984=CARTESIAN_POINT('Origin',(120.65,126.2,43.65));
#21985=CARTESIAN_POINT('',(120.65,127.,43.65));
#21986=CARTESIAN_POINT('',(120.65,126.2,44.45));
#21987=CARTESIAN_POINT('Origin',(139.7,127.,-31.75));
#21988=CARTESIAN_POINT('Origin',(120.65,123.0375,43.65));
#21989=CARTESIAN_POINT('',(120.65,123.0375,44.45));
#21990=CARTESIAN_POINT('Origin',(101.6,122.2375,44.45));
#21991=CARTESIAN_POINT('',(0.,0.,0.));
#21992=CARTESIAN_POINT('Origin',(15.2,-16.,21.975));
#21993=CARTESIAN_POINT('',(12.25,-16.,22.225));
#21994=CARTESIAN_POINT('Origin',(15.2,-16.,22.225));
#21995=CARTESIAN_POINT('',(12.75,-16.,21.725));
#21996=CARTESIAN_POINT('',(12.5,-16.,21.975));
#21997=CARTESIAN_POINT('Origin',(15.2,-16.,21.725));
#21998=CARTESIAN_POINT('Origin',(15.2,-16.,22.225));
#21999=CARTESIAN_POINT('',(12.75,-16.,19.525));
#22000=CARTESIAN_POINT('',(12.75,-16.,22.225));
#22001=CARTESIAN_POINT('Origin',(15.2,-16.,19.525));
#22002=CARTESIAN_POINT('Origin',(32.925,0.,22.225));
#22003=CARTESIAN_POINT('',(-2.525,-0.5,22.225));
#22004=CARTESIAN_POINT('',(32.925,-0.5,22.225));
#22005=CARTESIAN_POINT('',(24.0625,-0.5,22.225));
#22006=CARTESIAN_POINT('',(-2.525,-31.15,22.225));
#22007=CARTESIAN_POINT('',(-2.525,0.,22.225));
#22008=CARTESIAN_POINT('',(32.925,-31.15,22.225));
#22009=CARTESIAN_POINT('',(24.0625,-31.15,22.225));
#22010=CARTESIAN_POINT('',(32.925,0.,22.225));
#22011=CARTESIAN_POINT('Origin',(15.2,-16.,19.275));
#22012=CARTESIAN_POINT('',(12.25,-16.,19.025));
#22013=CARTESIAN_POINT('Origin',(15.2,-16.,19.025));
#22014=CARTESIAN_POINT('',(12.5,-16.,19.275));
#22015=CARTESIAN_POINT('Origin',(-2.525,0.,19.025));
#22016=CARTESIAN_POINT('',(32.925,-0.5,19.025));
#22017=CARTESIAN_POINT('',(-2.525,-0.5,19.025));
#22018=CARTESIAN_POINT('',(6.3375,-0.5,19.025));
#22019=CARTESIAN_POINT('',(32.925,-31.15,19.025));
#22020=CARTESIAN_POINT('',(32.925,0.,19.025));
#22021=CARTESIAN_POINT('',(-2.525,-31.15,19.025));
#22022=CARTESIAN_POINT('',(6.3375,-31.15,19.025));
#22023=CARTESIAN_POINT('',(-2.525,0.,19.025));
#22024=CARTESIAN_POINT('Origin',(24.0625,-0.25,-19.275));
#22025=CARTESIAN_POINT('',(32.925,-0.5,-19.025));
#22026=CARTESIAN_POINT('',(32.925,0.,-19.525));
#22027=CARTESIAN_POINT('',(32.925,-0.5,-19.025));
#22028=CARTESIAN_POINT('',(-2.525,0.,-19.525));
#22029=CARTESIAN_POINT('',(24.0625,0.,-19.525));
#22030=CARTESIAN_POINT('',(-2.525,-0.5,-19.025));
#22031=CARTESIAN_POINT('',(-2.525,0.,-19.525));
#22032=CARTESIAN_POINT('',(24.0625,-0.5,-19.025));
#22033=CARTESIAN_POINT('Origin',(32.925,-0.25,-17.725));
#22034=CARTESIAN_POINT('',(34.225,-0.5,-17.725));
#22035=CARTESIAN_POINT('',(34.725,0.,-17.725));
#22036=CARTESIAN_POINT('',(34.225,-0.5,-17.725));
#22037=CARTESIAN_POINT('Origin',(32.925,0.,-17.725));
#22038=CARTESIAN_POINT('Origin',(32.925,-0.5,-17.725));
#22039=CARTESIAN_POINT('Origin',(34.475,-0.25,8.8625));
#22040=CARTESIAN_POINT('',(34.225,-0.5,17.725));
#22041=CARTESIAN_POINT('',(34.725,0.,17.725));
#22042=CARTESIAN_POINT('',(34.225,-0.5,17.725));
#22043=CARTESIAN_POINT('',(34.725,0.,8.8625));
#22044=CARTESIAN_POINT('',(34.225,-0.5,8.8625));
#22045=CARTESIAN_POINT('Origin',(32.925,-0.25,17.725));
#22046=CARTESIAN_POINT('',(32.925,0.,19.525));
#22047=CARTESIAN_POINT('',(32.925,-0.5,19.025));
#22048=CARTESIAN_POINT('Origin',(32.925,0.,17.725));
#22049=CARTESIAN_POINT('Origin',(32.925,-0.5,17.725));
#22050=CARTESIAN_POINT('Origin',(6.3375,-0.25,19.275));
#22051=CARTESIAN_POINT('',(-2.525,0.,19.525));
#22052=CARTESIAN_POINT('',(-2.525,-0.5,19.025));
#22053=CARTESIAN_POINT('',(6.3375,0.,19.525));
#22054=CARTESIAN_POINT('Origin',(-2.525,-0.25,17.725));
#22055=CARTESIAN_POINT('',(-3.825,-0.5,17.725));
#22056=CARTESIAN_POINT('',(-4.325,0.,17.725));
#22057=CARTESIAN_POINT('',(-3.825,-0.5,17.725));
#22058=CARTESIAN_POINT('Origin',(-2.525,0.,17.725));
#22059=CARTESIAN_POINT('Origin',(-2.525,-0.5,17.725));
#22060=CARTESIAN_POINT('Origin',(-4.075,-0.25,-8.8625));
#22061=CARTESIAN_POINT('',(-3.825,-0.5,-17.725));
#22062=CARTESIAN_POINT('',(-4.325,0.,-17.725));
#22063=CARTESIAN_POINT('',(-3.825,-0.5,-17.725));
#22064=CARTESIAN_POINT('',(-4.325,0.,-8.8625));
#22065=CARTESIAN_POINT('',(-3.825,-0.5,-8.8625));
#22066=CARTESIAN_POINT('Origin',(-2.525,-0.25,-17.725));
#22067=CARTESIAN_POINT('Origin',(-2.525,0.,-17.725));
#22068=CARTESIAN_POINT('Origin',(-2.525,-0.5,-17.725));
#22069=CARTESIAN_POINT('Origin',(32.925,0.,17.725));
#22070=CARTESIAN_POINT('',(34.225,-31.15,17.725));
#22071=CARTESIAN_POINT('',(34.225,0.,17.725));
#22072=CARTESIAN_POINT('Origin',(32.925,-31.15,17.725));
#22073=CARTESIAN_POINT('Origin',(34.225,0.,17.725));
#22074=CARTESIAN_POINT('',(34.225,-31.15,-17.725));
#22075=CARTESIAN_POINT('',(34.225,0.,-17.725));
#22076=CARTESIAN_POINT('',(34.225,-31.15,8.8625));
#22077=CARTESIAN_POINT('Origin',(32.925,0.,-17.725));
#22078=CARTESIAN_POINT('',(32.925,-31.15,-19.025));
#22079=CARTESIAN_POINT('',(32.925,0.,-19.025));
#22080=CARTESIAN_POINT('Origin',(32.925,-31.15,-17.725));
#22081=CARTESIAN_POINT('Origin',(32.925,0.,-19.025));
#22082=CARTESIAN_POINT('',(-2.525,-31.15,-19.025));
#22083=CARTESIAN_POINT('',(-2.525,0.,-19.025));
#22084=CARTESIAN_POINT('',(24.0625,-31.15,-19.025));
#22085=CARTESIAN_POINT('Origin',(15.2,0.,0.));
#22086=CARTESIAN_POINT('',(36.925,0.,17.725));
#22087=CARTESIAN_POINT('',(32.925,0.,21.725));
#22088=CARTESIAN_POINT('Origin',(32.925,0.,17.725));
#22089=CARTESIAN_POINT('',(36.925,0.,-17.725));
#22090=CARTESIAN_POINT('',(36.925,0.,-8.8625));
#22091=CARTESIAN_POINT('',(32.925,0.,-21.725));
#22092=CARTESIAN_POINT('Origin',(32.925,0.,-17.725));
#22093=CARTESIAN_POINT('',(-2.525,0.,-21.725));
#22094=CARTESIAN_POINT('',(6.3375,0.,-21.725));
#22095=CARTESIAN_POINT('',(-6.525,0.,-17.725));
#22096=CARTESIAN_POINT('Origin',(-2.525,0.,-17.725));
#22097=CARTESIAN_POINT('',(-6.525,0.,17.725));
#22098=CARTESIAN_POINT('',(-6.525,0.,8.8625));
#22099=CARTESIAN_POINT('',(-2.525,0.,21.725));
#22100=CARTESIAN_POINT('Origin',(-2.525,0.,17.725));
#22101=CARTESIAN_POINT('',(24.0625,0.,21.725));
#22102=CARTESIAN_POINT('Origin',(32.925,-0.25,17.725));
#22103=CARTESIAN_POINT('',(37.425,-0.5,17.725));
#22104=CARTESIAN_POINT('',(37.425,-0.5,17.725));
#22105=CARTESIAN_POINT('',(32.925,0.,21.725));
#22106=CARTESIAN_POINT('Origin',(32.925,-0.5,17.725));
#22107=CARTESIAN_POINT('Origin',(37.175,-0.25,-8.8625));
#22108=CARTESIAN_POINT('',(37.425,-0.5,-17.725));
#22109=CARTESIAN_POINT('',(37.425,-0.5,-8.8625));
#22110=CARTESIAN_POINT('',(37.425,-0.5,-17.725));
#22111=CARTESIAN_POINT('Origin',(32.925,-0.25,-17.725));
#22112=CARTESIAN_POINT('',(32.925,-0.5,-22.225));
#22113=CARTESIAN_POINT('',(32.925,-0.5,-22.225));
#22114=CARTESIAN_POINT('Origin',(32.925,-0.5,-17.725));
#22115=CARTESIAN_POINT('Origin',(6.3375,-0.25,-21.975));
#22116=CARTESIAN_POINT('',(-2.525,-0.5,-22.225));
#22117=CARTESIAN_POINT('',(6.3375,-0.5,-22.225));
#22118=CARTESIAN_POINT('',(-2.525,-0.5,-22.225));
#22119=CARTESIAN_POINT('Origin',(-2.525,-0.25,-17.725));
#22120=CARTESIAN_POINT('',(-7.025,-0.5,-17.725));
#22121=CARTESIAN_POINT('',(-7.025,-0.5,-17.725));
#22122=CARTESIAN_POINT('Origin',(-2.525,-0.5,-17.725));
#22123=CARTESIAN_POINT('Origin',(-6.775,-0.25,8.8625));
#22124=CARTESIAN_POINT('',(-7.025,-0.5,17.725));
#22125=CARTESIAN_POINT('',(-7.025,-0.5,8.8625));
#22126=CARTESIAN_POINT('',(-7.025,-0.5,17.725));
#22127=CARTESIAN_POINT('Origin',(-2.525,-0.25,17.725));
#22128=CARTESIAN_POINT('',(-2.525,-0.5,22.225));
#22129=CARTESIAN_POINT('Origin',(-2.525,-0.5,17.725));
#22130=CARTESIAN_POINT('Origin',(24.0625,-0.25,21.975));
#22131=CARTESIAN_POINT('Origin',(-2.525,0.,-22.225));
#22132=CARTESIAN_POINT('',(32.925,-31.15,-22.225));
#22133=CARTESIAN_POINT('',(32.925,0.,-22.225));
#22134=CARTESIAN_POINT('',(-2.525,-31.15,-22.225));
#22135=CARTESIAN_POINT('',(6.3375,-31.15,-22.225));
#22136=CARTESIAN_POINT('',(-2.525,0.,-22.225));
#22137=CARTESIAN_POINT('Origin',(32.925,0.,-17.725));
#22138=CARTESIAN_POINT('',(37.425,-31.15,-17.725));
#22139=CARTESIAN_POINT('',(37.425,0.,-17.725));
#22140=CARTESIAN_POINT('Origin',(32.925,-31.15,-17.725));
#22141=CARTESIAN_POINT('Origin',(37.425,0.,-17.725));
#22142=CARTESIAN_POINT('',(37.425,-31.15,17.725));
#22143=CARTESIAN_POINT('',(37.425,0.,17.725));
#22144=CARTESIAN_POINT('',(37.425,-31.15,-8.8625));
#22145=CARTESIAN_POINT('Origin',(32.925,0.,17.725));
#22146=CARTESIAN_POINT('Origin',(32.925,-31.15,17.725));
#22147=CARTESIAN_POINT('Origin',(6.3375,-31.45,-21.925));
#22148=CARTESIAN_POINT('',(32.925,-31.75,-21.625));
#22149=CARTESIAN_POINT('',(32.925,-31.15,-22.225));
#22150=CARTESIAN_POINT('',(-2.525,-31.75,-21.625));
#22151=CARTESIAN_POINT('',(6.3375,-31.75,-21.625));
#22152=CARTESIAN_POINT('',(-2.525,-31.75,-21.625));
#22153=CARTESIAN_POINT('Origin',(32.925,-31.45,-17.725));
#22154=CARTESIAN_POINT('',(36.825,-31.75,-17.725));
#22155=CARTESIAN_POINT('',(37.425,-31.15,-17.725));
#22156=CARTESIAN_POINT('Origin',(32.925,-31.75,-17.725));
#22157=CARTESIAN_POINT('Origin',(37.125,-31.45,-8.8625));
#22158=CARTESIAN_POINT('',(36.825,-31.75,17.725));
#22159=CARTESIAN_POINT('',(37.425,-31.15,17.725));
#22160=CARTESIAN_POINT('',(36.825,-31.75,-8.8625));
#22161=CARTESIAN_POINT('Origin',(32.925,-31.45,17.725));
#22162=CARTESIAN_POINT('',(32.925,-31.75,21.625));
#22163=CARTESIAN_POINT('',(32.925,-31.15,22.225));
#22164=CARTESIAN_POINT('Origin',(32.925,-31.75,17.725));
#22165=CARTESIAN_POINT('Origin',(24.0625,-31.45,21.925));
#22166=CARTESIAN_POINT('',(-2.525,-31.75,21.625));
#22167=CARTESIAN_POINT('',(-2.525,-31.15,22.225));
#22168=CARTESIAN_POINT('',(24.0625,-31.75,21.625));
#22169=CARTESIAN_POINT('Origin',(-2.525,-31.45,17.725));
#22170=CARTESIAN_POINT('',(-7.025,-31.15,17.725));
#22171=CARTESIAN_POINT('',(-6.425,-31.75,17.725));
#22172=CARTESIAN_POINT('',(-7.025,-31.15,17.725));
#22173=CARTESIAN_POINT('Origin',(-2.525,-31.75,17.725));
#22174=CARTESIAN_POINT('Origin',(-2.525,-31.15,17.725));
#22175=CARTESIAN_POINT('Origin',(-6.725,-31.45,8.8625));
#22176=CARTESIAN_POINT('',(-7.025,-31.15,-17.725));
#22177=CARTESIAN_POINT('',(-6.425,-31.75,-17.725));
#22178=CARTESIAN_POINT('',(-7.025,-31.15,-17.725));
#22179=CARTESIAN_POINT('',(-6.425,-31.75,8.8625));
#22180=CARTESIAN_POINT('',(-7.025,-31.15,8.8625));
#22181=CARTESIAN_POINT('Origin',(-2.525,-31.45,-17.725));
#22182=CARTESIAN_POINT('Origin',(-2.525,-31.75,-17.725));
#22183=CARTESIAN_POINT('Origin',(-2.525,-31.15,-17.725));
#22184=CARTESIAN_POINT('Origin',(15.2,-31.75,0.));
#22185=CARTESIAN_POINT('',(34.825,-31.75,-17.725));
#22186=CARTESIAN_POINT('',(34.825,-31.75,17.725));
#22187=CARTESIAN_POINT('',(34.825,-31.75,8.8625));
#22188=CARTESIAN_POINT('',(32.925,-31.75,-19.625));
#22189=CARTESIAN_POINT('Origin',(32.925,-31.75,-17.725));
#22190=CARTESIAN_POINT('',(-2.525,-31.75,-19.625));
#22191=CARTESIAN_POINT('',(24.0625,-31.75,-19.625));
#22192=CARTESIAN_POINT('',(-4.425,-31.75,-17.725));
#22193=CARTESIAN_POINT('Origin',(-2.525,-31.75,-17.725));
#22194=CARTESIAN_POINT('',(-4.425,-31.75,17.725));
#22195=CARTESIAN_POINT('',(-4.425,-31.75,-8.8625));
#22196=CARTESIAN_POINT('',(-2.525,-31.75,19.625));
#22197=CARTESIAN_POINT('Origin',(-2.525,-31.75,17.725));
#22198=CARTESIAN_POINT('',(32.925,-31.75,19.625));
#22199=CARTESIAN_POINT('',(6.3375,-31.75,19.625));
#22200=CARTESIAN_POINT('Origin',(32.925,-31.75,17.725));
#22201=CARTESIAN_POINT('Origin',(34.525,-31.45,8.8625));
#22202=CARTESIAN_POINT('',(34.225,-31.15,-17.725));
#22203=CARTESIAN_POINT('',(34.825,-31.75,17.725));
#22204=CARTESIAN_POINT('Origin',(32.925,-31.45,-17.725));
#22205=CARTESIAN_POINT('',(32.925,-31.15,-19.025));
#22206=CARTESIAN_POINT('Origin',(24.0625,-31.45,-19.325));
#22207=CARTESIAN_POINT('',(-2.525,-31.15,-19.025));
#22208=CARTESIAN_POINT('Origin',(-2.525,-31.45,-17.725));
#22209=CARTESIAN_POINT('',(-3.825,-31.15,-17.725));
#22210=CARTESIAN_POINT('',(-3.825,-31.15,-17.725));
#22211=CARTESIAN_POINT('Origin',(-2.525,-31.15,-17.725));
#22212=CARTESIAN_POINT('Origin',(-4.125,-31.45,-8.8625));
#22213=CARTESIAN_POINT('',(-3.825,-31.15,17.725));
#22214=CARTESIAN_POINT('',(-3.825,-31.15,17.725));
#22215=CARTESIAN_POINT('',(-3.825,-31.15,-8.8625));
#22216=CARTESIAN_POINT('Origin',(-2.525,-31.45,17.725));
#22217=CARTESIAN_POINT('',(-2.525,-31.15,19.025));
#22218=CARTESIAN_POINT('Origin',(-2.525,-31.15,17.725));
#22219=CARTESIAN_POINT('Origin',(6.3375,-31.45,19.325));
#22220=CARTESIAN_POINT('',(32.925,-31.15,19.025));
#22221=CARTESIAN_POINT('Origin',(32.925,-31.45,17.725));
#22222=CARTESIAN_POINT('Origin',(-2.525,0.,-17.725));
#22223=CARTESIAN_POINT('',(-3.825,0.,-17.725));
#22224=CARTESIAN_POINT('Origin',(-2.525,0.,17.725));
#22225=CARTESIAN_POINT('',(-3.825,0.,17.725));
#22226=CARTESIAN_POINT('Origin',(-3.825,0.,-17.725));
#22227=CARTESIAN_POINT('Origin',(-2.525,0.,-17.725));
#22228=CARTESIAN_POINT('',(-7.025,0.,-17.725));
#22229=CARTESIAN_POINT('Origin',(-7.025,0.,17.725));
#22230=CARTESIAN_POINT('',(-7.025,0.,17.725));
#22231=CARTESIAN_POINT('Origin',(-2.525,0.,17.725));
#22232=CARTESIAN_POINT('',(0.,0.,0.));
#22233=CARTESIAN_POINT('Origin',(46.95,31.75,-20.8875));
#22234=CARTESIAN_POINT('',(41.25,31.75,-20.6375));
#22235=CARTESIAN_POINT('Origin',(46.95,31.75,-20.6375));
#22236=CARTESIAN_POINT('',(41.75,31.75,-21.1375));
#22237=CARTESIAN_POINT('',(41.5,31.75,-20.8875));
#22238=CARTESIAN_POINT('Origin',(46.95,31.75,-21.1375));
#22239=CARTESIAN_POINT('Origin',(-67.35,51.15,-20.6375));
#22240=CARTESIAN_POINT('',(-66.85,12.35,-20.6375));
#22241=CARTESIAN_POINT('',(-66.85,51.15,-20.6375));
#22242=CARTESIAN_POINT('',(-66.85,41.45,-20.6375));
#22243=CARTESIAN_POINT('',(109.85,12.35,-20.6375));
#22244=CARTESIAN_POINT('',(-67.35,12.35,-20.6375));
#22245=CARTESIAN_POINT('',(109.85,51.15,-20.6375));
#22246=CARTESIAN_POINT('',(109.85,41.45,-20.6375));
#22247=CARTESIAN_POINT('',(-67.35,51.15,-20.6375));
#22248=CARTESIAN_POINT('',(-22.25,31.75,-20.6375));
#22249=CARTESIAN_POINT('Origin',(-16.55,31.75,-20.6375));
#22250=CARTESIAN_POINT('',(9.50000000000001,31.75,-20.6375));
#22251=CARTESIAN_POINT('Origin',(15.2,31.75,-20.6375));
#22252=CARTESIAN_POINT('',(57.125,31.75,-20.6375));
#22253=CARTESIAN_POINT('Origin',(62.825,31.75,-20.6375));
#22254=CARTESIAN_POINT('',(25.375,31.75,-20.6375));
#22255=CARTESIAN_POINT('Origin',(31.075,31.75,-20.6375));
#22256=CARTESIAN_POINT('',(-6.375,31.75,-20.6375));
#22257=CARTESIAN_POINT('Origin',(-0.674999999999997,31.75,-20.6375));
#22258=CARTESIAN_POINT('Origin',(46.95,31.75,-25.4));
#22259=CARTESIAN_POINT('',(41.75,31.75,-24.9));
#22260=CARTESIAN_POINT('Origin',(46.95,31.75,-24.9));
#22261=CARTESIAN_POINT('',(41.75,31.75,-25.4));
#22262=CARTESIAN_POINT('Origin',(-16.55,31.75,-20.8875));
#22263=CARTESIAN_POINT('',(-21.75,31.75,-21.1375));
#22264=CARTESIAN_POINT('',(-22.,31.75,-20.8875));
#22265=CARTESIAN_POINT('Origin',(-16.55,31.75,-21.1375));
#22266=CARTESIAN_POINT('Origin',(-16.55,31.75,-25.4));
#22267=CARTESIAN_POINT('',(-21.75,31.75,-24.9));
#22268=CARTESIAN_POINT('Origin',(-16.55,31.75,-24.9));
#22269=CARTESIAN_POINT('',(-21.75,31.75,-25.4));
#22270=CARTESIAN_POINT('Origin',(-0.674999999999997,31.75,-20.8875));
#22271=CARTESIAN_POINT('',(-5.875,31.75,-21.1375));
#22272=CARTESIAN_POINT('',(-6.125,31.75,-20.8875));
#22273=CARTESIAN_POINT('Origin',(-0.674999999999997,31.75,-21.1375));
#22274=CARTESIAN_POINT('Origin',(-0.674999999999997,31.75,-25.4));
#22275=CARTESIAN_POINT('',(-5.875,31.75,-24.9));
#22276=CARTESIAN_POINT('Origin',(-0.674999999999997,31.75,-24.9));
#22277=CARTESIAN_POINT('',(-5.875,31.75,-25.4));
#22278=CARTESIAN_POINT('Origin',(15.2,31.75,-20.8875));
#22279=CARTESIAN_POINT('',(10.,31.75,-21.1375));
#22280=CARTESIAN_POINT('',(9.75000000000001,31.75,-20.8875));
#22281=CARTESIAN_POINT('Origin',(15.2,31.75,-21.1375));
#22282=CARTESIAN_POINT('Origin',(15.2,31.75,-25.4));
#22283=CARTESIAN_POINT('',(10.,31.75,-24.9));
#22284=CARTESIAN_POINT('Origin',(15.2,31.75,-24.9));
#22285=CARTESIAN_POINT('',(10.,31.75,-25.4));
#22286=CARTESIAN_POINT('Origin',(31.075,31.75,-20.8875));
#22287=CARTESIAN_POINT('',(25.875,31.75,-21.1375));
#22288=CARTESIAN_POINT('',(25.625,31.75,-20.8875));
#22289=CARTESIAN_POINT('Origin',(31.075,31.75,-21.1375));
#22290=CARTESIAN_POINT('Origin',(31.075,31.75,-25.4));
#22291=CARTESIAN_POINT('',(25.875,31.75,-24.9));
#22292=CARTESIAN_POINT('Origin',(31.075,31.75,-24.9));
#22293=CARTESIAN_POINT('',(25.875,31.75,-25.4));
#22294=CARTESIAN_POINT('Origin',(62.825,31.75,-20.8875));
#22295=CARTESIAN_POINT('',(57.625,31.75,-21.1375));
#22296=CARTESIAN_POINT('',(57.375,31.75,-20.8875));
#22297=CARTESIAN_POINT('Origin',(62.825,31.75,-21.1375));
#22298=CARTESIAN_POINT('Origin',(62.825,31.75,-25.4));
#22299=CARTESIAN_POINT('',(57.625,31.75,-24.9));
#22300=CARTESIAN_POINT('Origin',(62.825,31.75,-24.9));
#22301=CARTESIAN_POINT('',(57.625,31.75,-25.4));
#22302=CARTESIAN_POINT('Origin',(62.825,10.8625,0.));
#22303=CARTESIAN_POINT('',(57.125,11.1125,6.98048675513991E-16));
#22304=CARTESIAN_POINT('Origin',(62.825,11.1125,0.));
#22305=CARTESIAN_POINT('',(57.625,10.6125,-6.36816335556623E-16));
#22306=CARTESIAN_POINT('',(57.375,10.8625,6.67432505535307E-16));
#22307=CARTESIAN_POINT('Origin',(62.825,10.6125,0.));
#22308=CARTESIAN_POINT('Origin',(-67.35,11.1125,-19.4));
#22309=CARTESIAN_POINT('',(-66.85,11.1125,19.4));
#22310=CARTESIAN_POINT('',(-66.85,11.1125,-19.4));
#22311=CARTESIAN_POINT('',(-66.85,11.1125,-9.7));
#22312=CARTESIAN_POINT('',(109.85,11.1125,19.4));
#22313=CARTESIAN_POINT('',(-67.35,11.1125,19.4));
#22314=CARTESIAN_POINT('',(109.85,11.1125,-19.4));
#22315=CARTESIAN_POINT('',(109.85,11.1125,-9.7));
#22316=CARTESIAN_POINT('',(-67.35,11.1125,-19.4));
#22317=CARTESIAN_POINT('',(25.375,11.1125,6.98048675513991E-16));
#22318=CARTESIAN_POINT('Origin',(31.075,11.1125,0.));
#22319=CARTESIAN_POINT('',(-6.375,11.1125,6.98048675513991E-16));
#22320=CARTESIAN_POINT('Origin',(-0.674999999999997,11.1125,0.));
#22321=CARTESIAN_POINT('',(41.25,11.1125,6.98048675513991E-16));
#22322=CARTESIAN_POINT('Origin',(46.95,11.1125,0.));
#22323=CARTESIAN_POINT('',(-22.25,11.1125,6.98048675513991E-16));
#22324=CARTESIAN_POINT('Origin',(-16.55,11.1125,0.));
#22325=CARTESIAN_POINT('',(9.50000000000001,11.1125,6.98048675513991E-16));
#22326=CARTESIAN_POINT('Origin',(15.2,11.1125,0.));
#22327=CARTESIAN_POINT('',(-56.8,11.1125,1.04094977927525E-15));
#22328=CARTESIAN_POINT('Origin',(-48.3,11.1125,0.));
#22329=CARTESIAN_POINT('Origin',(62.825,6.35,0.));
#22330=CARTESIAN_POINT('',(57.625,6.85,6.36816335556623E-16));
#22331=CARTESIAN_POINT('Origin',(62.825,6.85,0.));
#22332=CARTESIAN_POINT('',(57.625,6.35,6.36816335556623E-16));
#22333=CARTESIAN_POINT('Origin',(-67.1,10.8625,-9.7));
#22334=CARTESIAN_POINT('',(-67.35,10.6125,19.4));
#22335=CARTESIAN_POINT('',(-67.35,10.6125,19.4));
#22336=CARTESIAN_POINT('',(-67.35,10.6125,-19.4));
#22337=CARTESIAN_POINT('',(-66.85,11.1125,-19.4));
#22338=CARTESIAN_POINT('',(-67.35,10.6125,-9.7));
#22339=CARTESIAN_POINT('Origin',(-67.1,12.35,19.4));
#22340=CARTESIAN_POINT('',(-67.35,12.35,21.1375));
#22341=CARTESIAN_POINT('',(-66.85,12.35,20.6375));
#22342=CARTESIAN_POINT('',(-67.35,12.35,21.1375));
#22343=CARTESIAN_POINT('Origin',(-66.85,12.35,19.4));
#22344=CARTESIAN_POINT('Origin',(-67.35,12.35,19.4));
#22345=CARTESIAN_POINT('Origin',(-67.1,22.05,20.8875));
#22346=CARTESIAN_POINT('',(-67.35,51.15,21.1375));
#22347=CARTESIAN_POINT('',(-66.85,51.15,20.6375));
#22348=CARTESIAN_POINT('',(-67.35,51.15,21.1375));
#22349=CARTESIAN_POINT('',(-66.85,22.05,20.6375));
#22350=CARTESIAN_POINT('',(-67.35,22.05,21.1375));
#22351=CARTESIAN_POINT('Origin',(-67.1,51.15,19.4));
#22352=CARTESIAN_POINT('',(-67.35,52.8875,19.4));
#22353=CARTESIAN_POINT('',(-66.85,52.3875,19.4));
#22354=CARTESIAN_POINT('',(-67.35,52.8875,19.4));
#22355=CARTESIAN_POINT('Origin',(-66.85,51.15,19.4));
#22356=CARTESIAN_POINT('Origin',(-67.35,51.15,19.4));
#22357=CARTESIAN_POINT('Origin',(-67.1,52.6375,9.7));
#22358=CARTESIAN_POINT('',(-67.35,52.8875,-19.4));
#22359=CARTESIAN_POINT('',(-66.85,52.3875,-19.4));
#22360=CARTESIAN_POINT('',(-67.35,52.8875,-19.4));
#22361=CARTESIAN_POINT('',(-66.85,52.3875,9.7));
#22362=CARTESIAN_POINT('',(-67.35,52.8875,9.7));
#22363=CARTESIAN_POINT('Origin',(-67.1,51.15,-19.4));
#22364=CARTESIAN_POINT('',(-67.35,51.15,-21.1375));
#22365=CARTESIAN_POINT('',(-67.35,51.15,-21.1375));
#22366=CARTESIAN_POINT('Origin',(-66.85,51.15,-19.4));
#22367=CARTESIAN_POINT('Origin',(-67.35,51.15,-19.4));
#22368=CARTESIAN_POINT('Origin',(-67.1,41.45,-20.8875));
#22369=CARTESIAN_POINT('',(-67.35,12.35,-21.1375));
#22370=CARTESIAN_POINT('',(-67.35,12.35,-21.1375));
#22371=CARTESIAN_POINT('',(-67.35,41.45,-21.1375));
#22372=CARTESIAN_POINT('Origin',(-67.1,12.35,-19.4));
#22373=CARTESIAN_POINT('Origin',(-66.85,12.35,-19.4));
#22374=CARTESIAN_POINT('Origin',(-67.35,12.35,-19.4));
#22375=CARTESIAN_POINT('Origin',(-67.35,51.15,-19.4));
#22376=CARTESIAN_POINT('',(109.85,52.3875,-19.4));
#22377=CARTESIAN_POINT('Origin',(109.85,51.15,-19.4));
#22378=CARTESIAN_POINT('',(-67.35,52.3875,-19.4));
#22379=CARTESIAN_POINT('Origin',(-67.35,12.35,-19.4));
#22380=CARTESIAN_POINT('Origin',(109.85,12.35,-19.4));
#22381=CARTESIAN_POINT('Origin',(-67.35,31.75,0.));
#22382=CARTESIAN_POINT('',(-67.35,12.35,-24.9));
#22383=CARTESIAN_POINT('',(-67.35,51.15,-24.9));
#22384=CARTESIAN_POINT('',(-67.35,22.05,-24.9));
#22385=CARTESIAN_POINT('',(-67.35,6.85,-19.4));
#22386=CARTESIAN_POINT('Origin',(-67.35,12.35,-19.4));
#22387=CARTESIAN_POINT('',(-67.35,6.85,19.4));
#22388=CARTESIAN_POINT('',(-67.35,6.85,9.7));
#22389=CARTESIAN_POINT('',(-67.35,12.35,24.9));
#22390=CARTESIAN_POINT('Origin',(-67.35,12.35,19.4));
#22391=CARTESIAN_POINT('',(-67.35,51.15,24.9));
#22392=CARTESIAN_POINT('',(-67.35,41.45,24.9));
#22393=CARTESIAN_POINT('',(-67.35,56.65,19.4));
#22394=CARTESIAN_POINT('Origin',(-67.35,51.15,19.4));
#22395=CARTESIAN_POINT('',(-67.35,56.65,-19.4));
#22396=CARTESIAN_POINT('',(-67.35,56.65,-9.7));
#22397=CARTESIAN_POINT('Origin',(-67.35,51.15,-19.4));
#22398=CARTESIAN_POINT('Origin',(-48.3,10.8625,0.));
#22399=CARTESIAN_POINT('',(-56.3,10.6125,-9.79717439317882E-16));
#22400=CARTESIAN_POINT('',(-56.55,10.8625,1.01033360929657E-15));
#22401=CARTESIAN_POINT('Origin',(-48.3,10.6125,0.));
#22402=CARTESIAN_POINT('Origin',(-48.3,6.35,0.));
#22403=CARTESIAN_POINT('',(-56.3,6.85,9.79717439317882E-16));
#22404=CARTESIAN_POINT('Origin',(-48.3,6.85,0.));
#22405=CARTESIAN_POINT('',(-56.3,6.35,9.79717439317882E-16));
#22406=CARTESIAN_POINT('Origin',(31.075,10.8625,0.));
#22407=CARTESIAN_POINT('',(25.875,10.6125,-6.36816335556624E-16));
#22408=CARTESIAN_POINT('',(25.625,10.8625,6.67432505535307E-16));
#22409=CARTESIAN_POINT('Origin',(31.075,10.6125,0.));
#22410=CARTESIAN_POINT('Origin',(31.075,6.35,0.));
#22411=CARTESIAN_POINT('',(25.875,6.85,6.36816335556624E-16));
#22412=CARTESIAN_POINT('Origin',(31.075,6.85,0.));
#22413=CARTESIAN_POINT('',(25.875,6.35,6.36816335556624E-16));
#22414=CARTESIAN_POINT('Origin',(15.2,10.8625,0.));
#22415=CARTESIAN_POINT('',(10.,10.6125,-6.36816335556623E-16));
#22416=CARTESIAN_POINT('',(9.75000000000001,10.8625,6.67432505535307E-16));
#22417=CARTESIAN_POINT('Origin',(15.2,10.6125,0.));
#22418=CARTESIAN_POINT('Origin',(15.2,6.35,0.));
#22419=CARTESIAN_POINT('',(10.,6.85,6.36816335556623E-16));
#22420=CARTESIAN_POINT('Origin',(15.2,6.85,0.));
#22421=CARTESIAN_POINT('',(10.,6.35,6.36816335556623E-16));
#22422=CARTESIAN_POINT('Origin',(-0.674999999999997,10.8625,0.));
#22423=CARTESIAN_POINT('',(-5.875,10.6125,-6.36816335556624E-16));
#22424=CARTESIAN_POINT('',(-6.125,10.8625,6.67432505535308E-16));
#22425=CARTESIAN_POINT('Origin',(-0.674999999999997,10.6125,0.));
#22426=CARTESIAN_POINT('Origin',(-0.674999999999997,6.35,0.));
#22427=CARTESIAN_POINT('',(-5.875,6.85,6.36816335556624E-16));
#22428=CARTESIAN_POINT('Origin',(-0.674999999999997,6.85,0.));
#22429=CARTESIAN_POINT('',(-5.875,6.35,6.36816335556624E-16));
#22430=CARTESIAN_POINT('Origin',(-16.55,10.8625,0.));
#22431=CARTESIAN_POINT('',(-21.75,10.6125,-6.36816335556624E-16));
#22432=CARTESIAN_POINT('',(-22.,10.8625,6.67432505535308E-16));
#22433=CARTESIAN_POINT('Origin',(-16.55,10.6125,0.));
#22434=CARTESIAN_POINT('Origin',(-16.55,6.35,0.));
#22435=CARTESIAN_POINT('',(-21.75,6.85,6.36816335556624E-16));
#22436=CARTESIAN_POINT('Origin',(-16.55,6.85,0.));
#22437=CARTESIAN_POINT('',(-21.75,6.35,6.36816335556624E-16));
#22438=CARTESIAN_POINT('Origin',(46.95,10.8625,0.));
#22439=CARTESIAN_POINT('',(41.75,10.6125,-6.36816335556623E-16));
#22440=CARTESIAN_POINT('',(41.5,10.8625,6.67432505535307E-16));
#22441=CARTESIAN_POINT('Origin',(46.95,10.6125,0.));
#22442=CARTESIAN_POINT('Origin',(46.95,6.35,0.));
#22443=CARTESIAN_POINT('',(41.75,6.85,6.36816335556623E-16));
#22444=CARTESIAN_POINT('Origin',(46.95,6.85,0.));
#22445=CARTESIAN_POINT('',(41.75,6.35,6.36816335556623E-16));
#22446=CARTESIAN_POINT('Origin',(-48.3,6.6,0.));
#22447=CARTESIAN_POINT('',(-56.8,6.35,-1.04094977927525E-15));
#22448=CARTESIAN_POINT('Origin',(-48.3,6.35,0.));
#22449=CARTESIAN_POINT('',(-56.55,6.6,-1.01033360929657E-15));
#22450=CARTESIAN_POINT('Origin',(-67.35,6.35,19.4));
#22451=CARTESIAN_POINT('',(-66.85,6.35,-19.4));
#22452=CARTESIAN_POINT('',(-66.85,6.35,19.4));
#22453=CARTESIAN_POINT('',(-66.85,6.35,9.7));
#22454=CARTESIAN_POINT('',(109.85,6.35,-19.4));
#22455=CARTESIAN_POINT('',(-67.35,6.35,-19.4));
#22456=CARTESIAN_POINT('',(109.85,6.35,19.4));
#22457=CARTESIAN_POINT('',(109.85,6.35,9.7));
#22458=CARTESIAN_POINT('',(-67.35,6.35,19.4));
#22459=CARTESIAN_POINT('',(57.125,6.35,-6.98048675513991E-16));
#22460=CARTESIAN_POINT('Origin',(62.825,6.35,0.));
#22461=CARTESIAN_POINT('',(9.50000000000001,6.35,-6.98048675513991E-16));
#22462=CARTESIAN_POINT('Origin',(15.2,6.35,0.));
#22463=CARTESIAN_POINT('',(-22.25,6.35,-6.98048675513991E-16));
#22464=CARTESIAN_POINT('Origin',(-16.55,6.35,0.));
#22465=CARTESIAN_POINT('',(41.25,6.35,-6.98048675513991E-16));
#22466=CARTESIAN_POINT('Origin',(46.95,6.35,0.));
#22467=CARTESIAN_POINT('',(-6.375,6.35,-6.98048675513991E-16));
#22468=CARTESIAN_POINT('Origin',(-0.674999999999997,6.35,0.));
#22469=CARTESIAN_POINT('',(25.375,6.35,-6.98048675513991E-16));
#22470=CARTESIAN_POINT('Origin',(31.075,6.35,0.));
#22471=CARTESIAN_POINT('Origin',(62.825,6.6,0.));
#22472=CARTESIAN_POINT('',(57.375,6.6,-6.67432505535307E-16));
#22473=CARTESIAN_POINT('Origin',(31.075,6.6,0.));
#22474=CARTESIAN_POINT('',(25.625,6.6,-6.67432505535307E-16));
#22475=CARTESIAN_POINT('Origin',(15.2,6.6,0.));
#22476=CARTESIAN_POINT('',(9.75000000000001,6.6,-6.67432505535307E-16));
#22477=CARTESIAN_POINT('Origin',(-0.674999999999997,6.6,0.));
#22478=CARTESIAN_POINT('',(-6.125,6.6,-6.67432505535308E-16));
#22479=CARTESIAN_POINT('Origin',(-16.55,6.6,0.));
#22480=CARTESIAN_POINT('',(-22.,6.6,-6.67432505535308E-16));
#22481=CARTESIAN_POINT('Origin',(46.95,6.6,0.));
#22482=CARTESIAN_POINT('',(41.5,6.6,-6.67432505535307E-16));
#22483=CARTESIAN_POINT('Origin',(-67.1,22.05,-25.15));
#22484=CARTESIAN_POINT('',(-66.85,51.15,-25.4));
#22485=CARTESIAN_POINT('',(-67.35,51.15,-24.9));
#22486=CARTESIAN_POINT('',(-66.85,12.35,-25.4));
#22487=CARTESIAN_POINT('',(-66.85,22.05,-25.4));
#22488=CARTESIAN_POINT('',(-66.85,12.35,-25.4));
#22489=CARTESIAN_POINT('Origin',(-67.1,51.15,-19.4));
#22490=CARTESIAN_POINT('',(-66.85,57.15,-19.4));
#22491=CARTESIAN_POINT('',(-67.35,56.65,-19.4));
#22492=CARTESIAN_POINT('Origin',(-66.85,51.15,-19.4));
#22493=CARTESIAN_POINT('Origin',(-67.1,56.9,-9.7));
#22494=CARTESIAN_POINT('',(-66.85,57.15,19.4));
#22495=CARTESIAN_POINT('',(-67.35,56.65,19.4));
#22496=CARTESIAN_POINT('',(-66.85,57.15,-9.7));
#22497=CARTESIAN_POINT('Origin',(-67.1,51.15,19.4));
#22498=CARTESIAN_POINT('',(-66.85,51.15,25.4));
#22499=CARTESIAN_POINT('',(-67.35,51.15,24.9));
#22500=CARTESIAN_POINT('Origin',(-66.85,51.15,19.4));
#22501=CARTESIAN_POINT('Origin',(-67.1,41.45,25.15));
#22502=CARTESIAN_POINT('',(-66.85,12.35,25.4));
#22503=CARTESIAN_POINT('',(-67.35,12.35,24.9));
#22504=CARTESIAN_POINT('',(-66.85,41.45,25.4));
#22505=CARTESIAN_POINT('Origin',(-67.1,12.35,19.4));
#22506=CARTESIAN_POINT('',(-67.35,6.85,19.4));
#22507=CARTESIAN_POINT('Origin',(-66.85,12.35,19.4));
#22508=CARTESIAN_POINT('Origin',(-67.1,6.6,9.7));
#22509=CARTESIAN_POINT('',(-67.35,6.85,-19.4));
#22510=CARTESIAN_POINT('Origin',(-67.1,12.35,-19.4));
#22511=CARTESIAN_POINT('Origin',(-66.85,12.35,-19.4));
#22512=CARTESIAN_POINT('Origin',(-67.35,12.35,19.4));
#22513=CARTESIAN_POINT('',(109.85,12.35,25.4));
#22514=CARTESIAN_POINT('Origin',(109.85,12.35,19.4));
#22515=CARTESIAN_POINT('',(-67.35,12.35,25.4));
#22516=CARTESIAN_POINT('Origin',(-67.35,12.35,-19.4));
#22517=CARTESIAN_POINT('',(109.85,12.35,-25.4));
#22518=CARTESIAN_POINT('',(-67.35,12.35,-25.4));
#22519=CARTESIAN_POINT('Origin',(109.85,12.35,-19.4));
#22520=CARTESIAN_POINT('Origin',(-67.35,12.35,-25.4));
#22521=CARTESIAN_POINT('',(109.85,51.15,-25.4));
#22522=CARTESIAN_POINT('',(-67.35,51.15,-25.4));
#22523=CARTESIAN_POINT('',(109.85,22.05,-25.4));
#22524=CARTESIAN_POINT('',(57.125,31.75,-25.4));
#22525=CARTESIAN_POINT('Origin',(62.825,31.75,-25.4));
#22526=CARTESIAN_POINT('',(9.50000000000001,31.75,-25.4));
#22527=CARTESIAN_POINT('Origin',(15.2,31.75,-25.4));
#22528=CARTESIAN_POINT('',(-22.25,31.75,-25.4));
#22529=CARTESIAN_POINT('Origin',(-16.55,31.75,-25.4));
#22530=CARTESIAN_POINT('',(41.25,31.75,-25.4));
#22531=CARTESIAN_POINT('Origin',(46.95,31.75,-25.4));
#22532=CARTESIAN_POINT('',(-6.375,31.75,-25.4));
#22533=CARTESIAN_POINT('Origin',(-0.674999999999997,31.75,-25.4));
#22534=CARTESIAN_POINT('',(25.375,31.75,-25.4));
#22535=CARTESIAN_POINT('Origin',(31.075,31.75,-25.4));
#22536=CARTESIAN_POINT('Origin',(62.825,31.75,-25.15));
#22537=CARTESIAN_POINT('',(57.375,31.75,-25.15));
#22538=CARTESIAN_POINT('Origin',(31.075,31.75,-25.15));
#22539=CARTESIAN_POINT('',(25.625,31.75,-25.15));
#22540=CARTESIAN_POINT('Origin',(15.2,31.75,-25.15));
#22541=CARTESIAN_POINT('',(9.75000000000001,31.75,-25.15));
#22542=CARTESIAN_POINT('Origin',(-0.674999999999997,31.75,-25.15));
#22543=CARTESIAN_POINT('',(-6.125,31.75,-25.15));
#22544=CARTESIAN_POINT('Origin',(-16.55,31.75,-25.15));
#22545=CARTESIAN_POINT('',(-22.,31.75,-25.15));
#22546=CARTESIAN_POINT('Origin',(46.95,31.75,-25.15));
#22547=CARTESIAN_POINT('',(41.5,31.75,-25.15));
#22548=CARTESIAN_POINT('Origin',(110.15,6.65,9.7));
#22549=CARTESIAN_POINT('',(110.45,6.95,-19.4));
#22550=CARTESIAN_POINT('',(109.85,6.35,-19.4));
#22551=CARTESIAN_POINT('',(110.45,6.95,19.4));
#22552=CARTESIAN_POINT('',(110.45,6.95,9.7));
#22553=CARTESIAN_POINT('',(110.45,6.95,19.4));
#22554=CARTESIAN_POINT('Origin',(110.15,12.35,-19.4));
#22555=CARTESIAN_POINT('',(110.45,12.35,-24.8));
#22556=CARTESIAN_POINT('',(109.85,12.35,-25.4));
#22557=CARTESIAN_POINT('Origin',(110.45,12.35,-19.4));
#22558=CARTESIAN_POINT('Origin',(110.15,22.05,-25.1));
#22559=CARTESIAN_POINT('',(110.45,51.15,-24.8));
#22560=CARTESIAN_POINT('',(109.85,51.15,-25.4));
#22561=CARTESIAN_POINT('',(110.45,22.05,-24.8));
#22562=CARTESIAN_POINT('Origin',(110.15,51.15,-19.4));
#22563=CARTESIAN_POINT('',(109.85,57.15,-19.4));
#22564=CARTESIAN_POINT('',(110.45,56.55,-19.4));
#22565=CARTESIAN_POINT('',(109.85,57.15,-19.4));
#22566=CARTESIAN_POINT('Origin',(110.45,51.15,-19.4));
#22567=CARTESIAN_POINT('Origin',(109.85,51.15,-19.4));
#22568=CARTESIAN_POINT('Origin',(110.15,56.85,-9.7));
#22569=CARTESIAN_POINT('',(109.85,57.15,19.4));
#22570=CARTESIAN_POINT('',(110.45,56.55,19.4));
#22571=CARTESIAN_POINT('',(109.85,57.15,19.4));
#22572=CARTESIAN_POINT('',(110.45,56.55,-9.7));
#22573=CARTESIAN_POINT('',(109.85,57.15,-9.7));
#22574=CARTESIAN_POINT('Origin',(110.15,51.15,19.4));
#22575=CARTESIAN_POINT('',(109.85,51.15,25.4));
#22576=CARTESIAN_POINT('',(110.45,51.15,24.8));
#22577=CARTESIAN_POINT('',(109.85,51.15,25.4));
#22578=CARTESIAN_POINT('Origin',(110.45,51.15,19.4));
#22579=CARTESIAN_POINT('Origin',(109.85,51.15,19.4));
#22580=CARTESIAN_POINT('Origin',(110.15,41.45,25.1));
#22581=CARTESIAN_POINT('',(110.45,12.35,24.8));
#22582=CARTESIAN_POINT('',(109.85,12.35,25.4));
#22583=CARTESIAN_POINT('',(110.45,41.45,24.8));
#22584=CARTESIAN_POINT('',(109.85,41.45,25.4));
#22585=CARTESIAN_POINT('Origin',(110.15,12.35,19.4));
#22586=CARTESIAN_POINT('Origin',(110.45,12.35,19.4));
#22587=CARTESIAN_POINT('Origin',(-67.35,51.15,-19.4));
#22588=CARTESIAN_POINT('',(-67.35,57.15,-19.4));
#22589=CARTESIAN_POINT('Origin',(110.45,31.75,0.));
#22590=CARTESIAN_POINT('',(110.45,12.35,-21.2375));
#22591=CARTESIAN_POINT('',(110.45,51.15,-21.2375));
#22592=CARTESIAN_POINT('',(110.45,41.45,-21.2375));
#22593=CARTESIAN_POINT('',(110.45,10.5125,-19.4));
#22594=CARTESIAN_POINT('Origin',(110.45,12.35,-19.4));
#22595=CARTESIAN_POINT('',(110.45,10.5125,19.4));
#22596=CARTESIAN_POINT('',(110.45,10.5125,-9.7));
#22597=CARTESIAN_POINT('',(110.45,12.35,21.2375));
#22598=CARTESIAN_POINT('Origin',(110.45,12.35,19.4));
#22599=CARTESIAN_POINT('',(110.45,51.15,21.2375));
#22600=CARTESIAN_POINT('',(110.45,22.05,21.2375));
#22601=CARTESIAN_POINT('',(110.45,52.9875,19.4));
#22602=CARTESIAN_POINT('Origin',(110.45,51.15,19.4));
#22603=CARTESIAN_POINT('',(110.45,52.9875,-19.4));
#22604=CARTESIAN_POINT('',(110.45,52.9875,9.7));
#22605=CARTESIAN_POINT('Origin',(110.45,51.15,-19.4));
#22606=CARTESIAN_POINT('Origin',(110.15,41.45,-20.9375));
#22607=CARTESIAN_POINT('',(109.85,12.35,-20.6375));
#22608=CARTESIAN_POINT('',(110.45,51.15,-21.2375));
#22609=CARTESIAN_POINT('Origin',(110.15,12.35,-19.4));
#22610=CARTESIAN_POINT('',(109.85,11.1125,-19.4));
#22611=CARTESIAN_POINT('Origin',(110.15,10.8125,-9.7));
#22612=CARTESIAN_POINT('',(109.85,11.1125,19.4));
#22613=CARTESIAN_POINT('Origin',(110.15,12.35,19.4));
#22614=CARTESIAN_POINT('',(109.85,12.35,20.6375));
#22615=CARTESIAN_POINT('',(109.85,12.35,20.6375));
#22616=CARTESIAN_POINT('Origin',(109.85,12.35,19.4));
#22617=CARTESIAN_POINT('Origin',(110.15,22.05,20.9375));
#22618=CARTESIAN_POINT('',(109.85,51.15,20.6375));
#22619=CARTESIAN_POINT('',(109.85,51.15,20.6375));
#22620=CARTESIAN_POINT('',(109.85,22.05,20.6375));
#22621=CARTESIAN_POINT('Origin',(110.15,51.15,19.4));
#22622=CARTESIAN_POINT('',(109.85,52.3875,19.4));
#22623=CARTESIAN_POINT('',(109.85,52.3875,19.4));
#22624=CARTESIAN_POINT('Origin',(109.85,51.15,19.4));
#22625=CARTESIAN_POINT('Origin',(110.15,52.6875,9.7));
#22626=CARTESIAN_POINT('',(109.85,52.3875,-19.4));
#22627=CARTESIAN_POINT('',(109.85,52.3875,9.7));
#22628=CARTESIAN_POINT('Origin',(110.15,51.15,-19.4));
#22629=CARTESIAN_POINT('Origin',(-67.35,12.35,19.4));
#22630=CARTESIAN_POINT('',(-67.35,12.35,20.6375));
#22631=CARTESIAN_POINT('Origin',(-67.35,52.3875,19.4));
#22632=CARTESIAN_POINT('',(-67.35,52.3875,19.4));
#22633=CARTESIAN_POINT('Origin',(-67.35,51.15,19.4));
#22634=CARTESIAN_POINT('',(-67.35,51.15,20.6375));
#22635=CARTESIAN_POINT('Origin',(-67.35,12.35,20.6375));
#22636=CARTESIAN_POINT('Origin',(-67.35,51.15,25.4));
#22637=CARTESIAN_POINT('',(-67.35,51.15,25.4));
#22638=CARTESIAN_POINT('Origin',(-67.35,51.15,19.4));
#22639=CARTESIAN_POINT('',(-67.35,57.15,19.4));
#22640=CARTESIAN_POINT('Origin',(-67.35,57.15,-19.4));
#22641=CARTESIAN_POINT('',(0.,0.,0.));
#22642=CARTESIAN_POINT('Ctrl Pts',(-67.9629497348173,6.06724190764723,-107.927825300627));
#22643=CARTESIAN_POINT('Ctrl Pts',(-67.9731885875005,6.09608154848999,-107.930287524609));
#22644=CARTESIAN_POINT('Ctrl Pts',(-68.0649619777051,6.35254287993133,-107.950374147766));
#22645=CARTESIAN_POINT('Ctrl Pts',(-68.1421523199026,6.56142467898147,-107.95));
#22646=CARTESIAN_POINT('Ctrl Pts',(-68.15,6.58309518948455,-107.95));
#22647=CARTESIAN_POINT('Ctrl Pts',(-68.0878080075958,6.02164898271821,-107.935082546577));
#22648=CARTESIAN_POINT('Ctrl Pts',(-68.0951549181554,6.04220422326524,-107.936123736671));
#22649=CARTESIAN_POINT('Ctrl Pts',(-68.1598746388879,6.22406166120123,-107.952418698047));
#22650=CARTESIAN_POINT('Ctrl Pts',(-68.2153859993183,6.37331286135221,-107.95));
#22651=CARTESIAN_POINT('Ctrl Pts',(-68.220972086323,6.38873012632303,-107.95));
#22652=CARTESIAN_POINT('Ctrl Pts',(-68.2126662803743,5.97605605778919,-107.942339792527));
#22653=CARTESIAN_POINT('Ctrl Pts',(-68.2170579361042,5.98825113903969,-107.942573272401));
#22654=CARTESIAN_POINT('Ctrl Pts',(-68.256721155555,6.09746416349077,-107.947668564864));
#22655=CARTESIAN_POINT('Ctrl Pts',(-68.288619678734,6.18520104372295,-107.95));
#22656=CARTESIAN_POINT('Ctrl Pts',(-68.291944172646,6.19436506316152,-107.95));
#22657=CARTESIAN_POINT('Ctrl Pts',(-68.3375245531529,5.93046313286018,-107.949597038478));
#22658=CARTESIAN_POINT('Ctrl Pts',(-68.3389416671525,5.93434379913925,-107.949642016394));
#22659=CARTESIAN_POINT('Ctrl Pts',(-68.351571877404,5.96893138250399,-107.950007869635));
#22660=CARTESIAN_POINT('Ctrl Pts',(-68.3618533581497,5.9970892260937,-107.95));
#22661=CARTESIAN_POINT('Ctrl Pts',(-68.3629162589689,6.,-107.95));
#22662=CARTESIAN_POINT('',(-68.15,6.58309518948455,-107.95));
#22663=CARTESIAN_POINT('',(-67.9629497348173,6.06724190764723,-107.927825300627));
#22664=CARTESIAN_POINT('Ctrl Pts',(-68.15,6.58309518948455,-107.95));
#22665=CARTESIAN_POINT('Ctrl Pts',(-68.1494585269681,6.58159997091316,-107.95));
#22666=CARTESIAN_POINT('Ctrl Pts',(-68.1489155383018,6.58010061545652,-107.949999490713));
#22667=CARTESIAN_POINT('Ctrl Pts',(-68.1483145418233,6.57844322897782,-107.949998224517));
#22668=CARTESIAN_POINT('Ctrl Pts',(-68.1476856008723,6.57670877916767,-107.949996899447));
#22669=CARTESIAN_POINT('Ctrl Pts',(-68.1469931402562,6.57480128397559,-107.949994750064));
#22670=CARTESIAN_POINT('Ctrl Pts',(-68.1461923150497,6.57259867099725,-107.949990938408));
#22671=CARTESIAN_POINT('Ctrl Pts',(-68.14536192547,6.57031474330575,-107.949986986036));
#22672=CARTESIAN_POINT('Ctrl Pts',(-68.1444150906044,6.56771369413093,-107.949981251966));
#22673=CARTESIAN_POINT('Ctrl Pts',(-68.1433221006719,6.56471475376682,-107.949972128052));
#22674=CARTESIAN_POINT('Ctrl Pts',(-68.1421797916733,6.56158049199336,-107.949962592439));
#22675=CARTESIAN_POINT('Ctrl Pts',(-68.1408779237317,6.55801185344092,-107.949949350216));
#22676=CARTESIAN_POINT('Ctrl Pts',(-68.1394032019918,6.55397281294346,-107.949929814341));
#22677=CARTESIAN_POINT('Ctrl Pts',(-68.1378429799736,6.54969960007502,-107.949909145831));
#22678=CARTESIAN_POINT('Ctrl Pts',(-68.1360893891363,6.54490016320098,-107.94988140751));
#22679=CARTESIAN_POINT('Ctrl Pts',(-68.1341478192351,6.53958932246212,-107.949842927308));
#22680=CARTESIAN_POINT('Ctrl Pts',(-68.1320491206422,6.53384868238592,-107.949801332955));
#22681=CARTESIAN_POINT('Ctrl Pts',(-68.1297309447041,6.52751095521807,-107.949747125478));
#22682=CARTESIAN_POINT('Ctrl Pts',(-68.1272221189739,6.52065461386469,-107.949675664339));
#22683=CARTESIAN_POINT('Ctrl Pts',(-68.1243771906191,6.51287974146469,-107.949594629686));
#22684=CARTESIAN_POINT('Ctrl Pts',(-68.1212873988534,6.50443878957247,-107.94949126786));
#22685=CARTESIAN_POINT('Ctrl Pts',(-68.1180187985553,6.49551117516029,-107.949360496118));
#22686=CARTESIAN_POINT('Ctrl Pts',(-68.1129443811809,6.48165128482386,-107.949157476373));
#22687=CARTESIAN_POINT('Ctrl Pts',(-68.1074407974137,6.46662336130254,-107.948887112081));
#22688=CARTESIAN_POINT('Ctrl Pts',(-68.1018027325981,6.45122664552437,-107.948546819801));
#22689=CARTESIAN_POINT('Ctrl Pts',(-68.0982065867868,6.44140610660473,-107.948329770034));
#22690=CARTESIAN_POINT('Ctrl Pts',(-68.0945567798222,6.43143836252592,-107.948084794035));
#22691=CARTESIAN_POINT('Ctrl Pts',(-68.0909213073327,6.42150762201437,-107.947815585253));
#22692=CARTESIAN_POINT('Ctrl Pts',(-68.0875130518738,6.4121975527848,-107.94756320202));
#22693=CARTESIAN_POINT('Ctrl Pts',(-68.0841178949647,6.40292137962132,-107.947289665233));
#22694=CARTESIAN_POINT('Ctrl Pts',(-68.0807745846575,6.39378372955142,-107.946999273444));
#22695=CARTESIAN_POINT('Ctrl Pts',(-68.0778535573511,6.38580022729814,-107.946745560128));
#22696=CARTESIAN_POINT('Ctrl Pts',(-68.0749721054198,6.37792247617486,-107.946479072676));
#22697=CARTESIAN_POINT('Ctrl Pts',(-68.0721398855605,6.37017591351234,-107.94620211164));
#22698=CARTESIAN_POINT('Ctrl Pts',(-68.069478336024,6.36289616077843,-107.945941840349));
#22699=CARTESIAN_POINT('Ctrl Pts',(-68.0668603435943,6.35573249576057,-107.945672384873));
#22700=CARTESIAN_POINT('Ctrl Pts',(-68.0642778922634,6.34866190828134,-107.945394066011));
#22701=CARTESIAN_POINT('Ctrl Pts',(-68.061799072167,6.34187505653043,-107.945126915811));
#22702=CARTESIAN_POINT('Ctrl Pts',(-68.0593530791771,6.3351742015672,-107.944851655774));
#22703=CARTESIAN_POINT('Ctrl Pts',(-68.0569163899697,6.32849354472908,-107.944566197081));
#22704=CARTESIAN_POINT('Ctrl Pts',(-68.0544290695812,6.32167407267163,-107.944274806934));
#22705=CARTESIAN_POINT('Ctrl Pts',(-68.0519486504824,6.314867926326,-107.943972484575));
#22706=CARTESIAN_POINT('Ctrl Pts',(-68.0494441127739,6.30798832458315,-107.943655160346));
#22707=CARTESIAN_POINT('Ctrl Pts',(-68.0468597289661,6.30088939718941,-107.943327719639));
#22708=CARTESIAN_POINT('Ctrl Pts',(-68.044249738723,6.29371244739674,-107.942984257085));
#22709=CARTESIAN_POINT('Ctrl Pts',(-68.0416004982127,6.286418578412,-107.9426219452));
#22710=CARTESIAN_POINT('Ctrl Pts',(-68.0388040332892,6.27871937228366,-107.942239498806));
#22711=CARTESIAN_POINT('Ctrl Pts',(-68.0359639561777,6.27089020577216,-107.941835999561));
#22712=CARTESIAN_POINT('Ctrl Pts',(-68.0330849632465,6.26294290518048,-107.941410686168));
#22713=CARTESIAN_POINT('Ctrl Pts',(-68.029986346019,6.2543893438785,-107.940952927695));
#22714=CARTESIAN_POINT('Ctrl Pts',(-68.0268428260038,6.24569938969678,-107.940469835404));
#22715=CARTESIAN_POINT('Ctrl Pts',(-68.0236813969289,6.23694695262799,-107.939964309648));
#22716=CARTESIAN_POINT('Ctrl Pts',(-68.0201202563992,6.22708791178246,-107.939394868356));
#22717=CARTESIAN_POINT('Ctrl Pts',(-68.0165366962784,6.21715035833223,-107.938796864838));
#22718=CARTESIAN_POINT('Ctrl Pts',(-68.0129916053749,6.20730341158762,-107.938180626381));
#22719=CARTESIAN_POINT('Ctrl Pts',(-68.0063167094922,6.18876302825924,-107.937020338068));
#22720=CARTESIAN_POINT('Ctrl Pts',(-67.9997811710551,6.17055030095131,-107.935793011526));
#22721=CARTESIAN_POINT('Ctrl Pts',(-67.9938677249504,6.15402777629214,-107.934616283726));
#22722=CARTESIAN_POINT('Ctrl Pts',(-67.9908424118573,6.14557486925642,-107.934014270964));
#22723=CARTESIAN_POINT('Ctrl Pts',(-67.9879803302263,6.13756600214908,-107.933426406399));
#22724=CARTESIAN_POINT('Ctrl Pts',(-67.9853349496579,6.13015493599242,-107.93286998997));
#22725=CARTESIAN_POINT('Ctrl Pts',(-67.9829511051419,6.12347656629908,-107.932368583757));
#22726=CARTESIAN_POINT('Ctrl Pts',(-67.9807434357073,6.11728427347295,-107.931892853576));
#22727=CARTESIAN_POINT('Ctrl Pts',(-67.9787370277375,6.11165176399922,-107.931453129965));
#22728=CARTESIAN_POINT('Ctrl Pts',(-67.9768605583099,6.10638402583844,-107.931041883635));
#22729=CARTESIAN_POINT('Ctrl Pts',(-67.9751602598371,6.10160632696771,-107.930662212486));
#22730=CARTESIAN_POINT('Ctrl Pts',(-67.973641409216,6.09733604160012,-107.930318939573));
#22731=CARTESIAN_POINT('Ctrl Pts',(-67.9722286436796,6.09336401702179,-107.929999642775));
#22732=CARTESIAN_POINT('Ctrl Pts',(-67.9709728991424,6.08983111529492,-107.92971186547));
#22733=CARTESIAN_POINT('Ctrl Pts',(-67.9698637164228,6.08670954431878,-107.929455527493));
#22734=CARTESIAN_POINT('Ctrl Pts',(-67.9687881735891,6.08368264601479,-107.929206963871));
#22735=CARTESIAN_POINT('Ctrl Pts',(-67.9678505353126,6.0810427906326,-107.928987991027));
#22736=CARTESIAN_POINT('Ctrl Pts',(-67.9670258484074,6.07872068925269,-107.928794234602));
#22737=CARTESIAN_POINT('Ctrl Pts',(-67.9662228305955,6.07645960233928,-107.928605569231));
#22738=CARTESIAN_POINT('Ctrl Pts',(-67.965526990813,6.07450002928015,-107.92844082974));
#22739=CARTESIAN_POINT('Ctrl Pts',(-67.9648991159876,6.07273187235018,-107.928291502419));
#22740=CARTESIAN_POINT('Ctrl Pts',(-67.9642908646836,6.07101897717607,-107.928146842155));
#22741=CARTESIAN_POINT('Ctrl Pts',(-67.9637464441481,6.06948585391573,-107.928016653354));
#22742=CARTESIAN_POINT('Ctrl Pts',(-67.9632138925135,6.06798592939913,-107.927888777429));
#22743=CARTESIAN_POINT('Ctrl Pts',(-67.9631256466347,6.06773738606814,-107.927867587891));
#22744=CARTESIAN_POINT('Ctrl Pts',(-67.9630376883609,6.06748964522963,-107.927846451563));
#22745=CARTESIAN_POINT('Ctrl Pts',(-67.9629497348173,6.06724190764723,-107.927825300627));
#22746=CARTESIAN_POINT('',(-68.3375245531529,5.93046313286018,-107.949597038478));
#22747=CARTESIAN_POINT('Ctrl Pts',(-68.3375245531529,5.93046313286018,-107.949597038478));
#22748=CARTESIAN_POINT('Ctrl Pts',(-68.2126662803743,5.97605605778919,-107.942339792527));
#22749=CARTESIAN_POINT('Ctrl Pts',(-68.0878080075958,6.02164898271821,-107.935082546577));
#22750=CARTESIAN_POINT('Ctrl Pts',(-67.9629497348173,6.06724190764723,-107.927825300627));
#22751=CARTESIAN_POINT('',(-68.3629162589689,6.,-107.95));
#22752=CARTESIAN_POINT('Ctrl Pts',(-68.3375245531529,5.93046313286018,-107.949597038478));
#22753=CARTESIAN_POINT('Ctrl Pts',(-68.3376484128971,5.9308023139938,-107.949600969674));
#22754=CARTESIAN_POINT('Ctrl Pts',(-68.3377738812747,5.93114590045188,-107.949604929021));
#22755=CARTESIAN_POINT('Ctrl Pts',(-68.3379336160622,5.93158332280906,-107.949609917176));
#22756=CARTESIAN_POINT('Ctrl Pts',(-68.3381007845541,5.93204110183711,-107.949615137469));
#22757=CARTESIAN_POINT('Ctrl Pts',(-68.3383053431287,5.93260127070113,-107.949621481053));
#22758=CARTESIAN_POINT('Ctrl Pts',(-68.3385647351012,5.93331159796506,-107.949629376639));
#22759=CARTESIAN_POINT('Ctrl Pts',(-68.3388581498122,5.93411509418272,-107.949638307837));
#22760=CARTESIAN_POINT('Ctrl Pts',(-68.3392217164581,5.93511069785869,-107.949649222747));
#22761=CARTESIAN_POINT('Ctrl Pts',(-68.3396564658575,5.93630123568428,-107.949661862757));
#22762=CARTESIAN_POINT('Ctrl Pts',(-68.3401321391992,5.93760384152248,-107.9496756926));
#22763=CARTESIAN_POINT('Ctrl Pts',(-68.3406925812451,5.93913858691483,-107.94969155866));
#22764=CARTESIAN_POINT('Ctrl Pts',(-68.3413155502779,5.94084456975624,-107.949708379169));
#22765=CARTESIAN_POINT('Ctrl Pts',(-68.3422472252028,5.94339593483566,-107.949733534908));
#22766=CARTESIAN_POINT('Ctrl Pts',(-68.3433170705235,5.94632569724319,-107.949760665181));
#22767=CARTESIAN_POINT('Ctrl Pts',(-68.3444107004731,5.94932062429725,-107.949785962922));
#22768=CARTESIAN_POINT('Ctrl Pts',(-68.3451482244235,5.95134034809204,-107.949803023254));
#22769=CARTESIAN_POINT('Ctrl Pts',(-68.3458954545405,5.95338666559863,-107.949819263662));
#22770=CARTESIAN_POINT('Ctrl Pts',(-68.3466257052537,5.95538649749514,-107.94983413399));
#22771=CARTESIAN_POINT('Ctrl Pts',(-68.3472620357263,5.95712912362719,-107.949847091791));
#22772=CARTESIAN_POINT('Ctrl Pts',(-68.3478852316262,5.9588357900753,-107.949859020331));
#22773=CARTESIAN_POINT('Ctrl Pts',(-68.3484914174909,5.96049588209922,-107.949869950646));
#22774=CARTESIAN_POINT('Ctrl Pts',(-68.3490583868923,5.96204857647187,-107.949880173838));
#22775=CARTESIAN_POINT('Ctrl Pts',(-68.3496102870568,5.9635600102806,-107.949889531659));
#22776=CARTESIAN_POINT('Ctrl Pts',(-68.3501598186094,5.96506496295212,-107.949898294404));
#22777=CARTESIAN_POINT('Ctrl Pts',(-68.3507102523001,5.96657238622828,-107.949907071534));
#22778=CARTESIAN_POINT('Ctrl Pts',(-68.3512614068472,5.96808178899628,-107.949915301922));
#22779=CARTESIAN_POINT('Ctrl Pts',(-68.351827369383,5.96963174796697,-107.949923146947));
#22780=CARTESIAN_POINT('Ctrl Pts',(-68.3524400984799,5.97130978299589,-107.949931640221));
#22781=CARTESIAN_POINT('Ctrl Pts',(-68.3530700019396,5.97303485537861,-107.949939665741));
#22782=CARTESIAN_POINT('Ctrl Pts',(-68.3537140997498,5.9747988021213,-107.949947074735));
#22783=CARTESIAN_POINT('Ctrl Pts',(-68.3544669504786,5.97686058306484,-107.949955734703));
#22784=CARTESIAN_POINT('Ctrl Pts',(-68.3552388966772,5.97897466126154,-107.949963524226));
#22785=CARTESIAN_POINT('Ctrl Pts',(-68.35600106939,5.98106197314171,-107.94997011252));
#22786=CARTESIAN_POINT('Ctrl Pts',(-68.3569159942254,5.98356761713371,-107.949978021219));
#22787=CARTESIAN_POINT('Ctrl Pts',(-68.3578152161114,5.98603025599149,-107.949984153345));
#22788=CARTESIAN_POINT('Ctrl Pts',(-68.3586312279608,5.98826500948253,-107.949988524155));
#22789=CARTESIAN_POINT('Ctrl Pts',(-68.3592601969867,5.98998752212431,-107.949991893107));
#22790=CARTESIAN_POINT('Ctrl Pts',(-68.3598389431586,5.9915724906411,-107.949994240505));
#22791=CARTESIAN_POINT('Ctrl Pts',(-68.3603434552782,5.99295415655121,-107.949995863006));
#22792=CARTESIAN_POINT('Ctrl Pts',(-68.360801738962,5.99420922044048,-107.949997336838));
#22793=CARTESIAN_POINT('Ctrl Pts',(-68.3611984503128,5.99529565802497,-107.949998223794));
#22794=CARTESIAN_POINT('Ctrl Pts',(-68.3615283752455,5.99619919007954,-107.949998796154));
#22795=CARTESIAN_POINT('Ctrl Pts',(-68.3618379571857,5.99704701083741,-107.949999333221));
#22796=CARTESIAN_POINT('Ctrl Pts',(-68.3620885335494,5.99773323519729,-107.94999959747));
#22797=CARTESIAN_POINT('Ctrl Pts',(-68.3622911398108,5.99828808589258,-107.949999755779));
#22798=CARTESIAN_POINT('Ctrl Pts',(-68.3624807303376,5.99880729213499,-107.949999903919));
#22799=CARTESIAN_POINT('Ctrl Pts',(-68.3626282304674,5.99921122722297,-107.949999958751));
#22800=CARTESIAN_POINT('Ctrl Pts',(-68.3627584528728,5.99956784464617,-107.949999984437));
#22801=CARTESIAN_POINT('Ctrl Pts',(-68.3628129524334,5.99971709310149,-107.949999995187));
#22802=CARTESIAN_POINT('Ctrl Pts',(-68.3628646310546,5.99985861598442,-107.95));
#22803=CARTESIAN_POINT('Ctrl Pts',(-68.3629162589689,6.,-107.95));
#22804=CARTESIAN_POINT('',(-68.2564581294845,6.29154759474227,-107.95));
#22805=CARTESIAN_POINT('Ctrl Pts',(-68.3375240385289,0.000402977856687192,
-102.019538276432));
#22806=CARTESIAN_POINT('Ctrl Pts',(-68.3380554670653,0.000386110454297121,
-102.01808299709));
#22807=CARTESIAN_POINT('Ctrl Pts',(-68.3397274021881,0.00032759961132862,
-102.013504598476));
#22808=CARTESIAN_POINT('Ctrl Pts',(-68.3466614877139,0.000156761636871131,
-101.994515645545));
#22809=CARTESIAN_POINT('Ctrl Pts',(-68.3522721650115,5.98098402742648E-5,
-101.979150165178));
#22810=CARTESIAN_POINT('Ctrl Pts',(-68.3583205753897,7.84684658830335E-6,
-101.962585741651));
#22811=CARTESIAN_POINT('Ctrl Pts',(-68.3618857180998,-2.66424903465483E-7,
-101.95282217754));
#22812=CARTESIAN_POINT('Ctrl Pts',(-68.3625619515145,-3.08148791101958E-32,
-101.950970277635));
#22813=CARTESIAN_POINT('Ctrl Pts',(-68.3629162589689,-3.08148791101958E-32,
-101.95));
#22814=CARTESIAN_POINT('Ctrl Pts',(-68.2126657709715,0.00766025835870256,
-101.973945350221));
#22815=CARTESIAN_POINT('Ctrl Pts',(-68.2143126524885,0.00757270097272666,
-101.969372165137));
#22816=CARTESIAN_POINT('Ctrl Pts',(-68.22076700718,0.00689140766747181,
-101.951555360678));
#22817=CARTESIAN_POINT('Ctrl Pts',(-68.239810705309,0.00496924519147893,
-101.899128861556));
#22818=CARTESIAN_POINT('Ctrl Pts',(-68.2597635158947,0.00276030806902361,
-101.844195710985));
#22819=CARTESIAN_POINT('Ctrl Pts',(-68.2772007293579,0.00110275965346496,
-101.796221353378));
#22820=CARTESIAN_POINT('Ctrl Pts',(-68.2878618278732,0.000211776221296321,
-101.76688366558));
#22821=CARTESIAN_POINT('Ctrl Pts',(-68.2908360008298,1.38777878078145E-16,
-101.758689629699));
#22822=CARTESIAN_POINT('Ctrl Pts',(-68.291944172646,1.38777878078145E-16,
-101.755634936838));
#22823=CARTESIAN_POINT('Ctrl Pts',(-68.0878075034141,0.0149175388607179,
-101.92835242401));
#22824=CARTESIAN_POINT('Ctrl Pts',(-68.0905626050853,0.0145270867471023,
-101.920644179277));
#22825=CARTESIAN_POINT('Ctrl Pts',(-68.098117885938,0.012488559345189,-101.899889546156));
#22826=CARTESIAN_POINT('Ctrl Pts',(-68.1376182455488,0.00738521760650383,
-101.792512628689));
#22827=CARTESIAN_POINT('Ctrl Pts',(-68.1645278494201,0.00313818569707965,
-101.718138514254));
#22828=CARTESIAN_POINT('Ctrl Pts',(-68.1976204498916,0.00103052104806465,
-101.626708713674));
#22829=CARTESIAN_POINT('Ctrl Pts',(-68.2165346834987,0.000408528025162008,
-101.573838723558));
#22830=CARTESIAN_POINT('Ctrl Pts',(-68.219110050145,2.77555756156289E-16,
-101.566408981763));
#22831=CARTESIAN_POINT('Ctrl Pts',(-68.220972086323,2.77555756156289E-16,
-101.561269873677));
#22832=CARTESIAN_POINT('Ctrl Pts',(-67.9629492358567,0.0221748193627333,
-101.882759497799));
#22833=CARTESIAN_POINT('Ctrl Pts',(-67.9667888156613,0.0212514803473293,
-101.871944602866));
#22834=CARTESIAN_POINT('Ctrl Pts',(-67.9787772078244,0.0180626748813272,
-101.837962280823));
#22835=CARTESIAN_POINT('Ctrl Pts',(-68.0292947457965,0.00869185796202674,
-101.697150420595));
#22836=CARTESIAN_POINT('Ctrl Pts',(-68.0708521582608,0.00330806576115239,
-101.583201284989));
#22837=CARTESIAN_POINT('Ctrl Pts',(-68.1158766125516,0.000432114042481723,
-101.460351904441));
#22838=CARTESIAN_POINT('Ctrl Pts',(-68.1423791757427,-1.45647633857201E-5,
-101.387901818545));
#22839=CARTESIAN_POINT('Ctrl Pts',(-68.1473840994603,4.16333634234434E-16,
-101.374128333826));
#22840=CARTESIAN_POINT('Ctrl Pts',(-68.15,4.16333634234434E-16,-101.366904810515));
#22841=CARTESIAN_POINT('',(-68.3629162589689,0.,-101.95));
#22842=CARTESIAN_POINT('',(-68.3375240385289,0.000402977856687192,-102.019538276432));
#22843=CARTESIAN_POINT('Ctrl Pts',(-68.3629162589689,0.,-101.95));
#22844=CARTESIAN_POINT('Ctrl Pts',(-68.3627923897953,0.,-101.950339218064));
#22845=CARTESIAN_POINT('Ctrl Pts',(-68.3626669120248,2.29080291819244E-8,
-101.950682841491));
#22846=CARTESIAN_POINT('Ctrl Pts',(-68.3625071684643,1.04590663241311E-7,
-101.951120307079));
#22847=CARTESIAN_POINT('Ctrl Pts',(-68.3623399907767,1.90074634203094E-7,
-101.95157813139));
#22848=CARTESIAN_POINT('Ctrl Pts',(-68.3621354236744,3.38991582082524E-7,
-101.952138352405));
#22849=CARTESIAN_POINT('Ctrl Pts',(-68.3618760240636,6.76277169375794E-7,
-101.952848741051));
#22850=CARTESIAN_POINT('Ctrl Pts',(-68.3615826009174,1.05780202161708E-6,
-101.953652306139));
#22851=CARTESIAN_POINT('Ctrl Pts',(-68.3612190270723,1.68218512989849E-6,
-101.954647990211));
#22852=CARTESIAN_POINT('Ctrl Pts',(-68.3607842715223,2.84078836632062E-6,
-101.955838617329));
#22853=CARTESIAN_POINT('Ctrl Pts',(-68.3603085925965,4.1084504882767E-6,
-101.957141317729));
#22854=CARTESIAN_POINT('Ctrl Pts',(-68.359748146621,6.0304302990709E-6,
-101.958676166968));
#22855=CARTESIAN_POINT('Ctrl Pts',(-68.3591251743955,8.98260877768564E-6,
-101.960382255277));
#22856=CARTESIAN_POINT('Ctrl Pts',(-68.3581934848705,1.33977554757658E-5,
-101.962933804996));
#22857=CARTESIAN_POINT('Ctrl Pts',(-68.3571236235583,2.02240548300365E-5,
-101.965863762444));
#22858=CARTESIAN_POINT('Ctrl Pts',(-68.3560299762102,2.96381295097348E-5,
-101.968858861994));
#22859=CARTESIAN_POINT('Ctrl Pts',(-68.3552924432318,3.59867852697833E-5,
-101.970878694707));
#22860=CARTESIAN_POINT('Ctrl Pts',(-68.3545452035351,4.34635720193775E-5,
-101.97292511089));
#22861=CARTESIAN_POINT('Ctrl Pts',(-68.3538149425036,5.1771638321263E-5,
-101.974925027172));
#22862=CARTESIAN_POINT('Ctrl Pts',(-68.3531786038672,5.90111641261043E-5,
-101.976667724572));
#22863=CARTESIAN_POINT('Ctrl Pts',(-68.3525553992048,6.68631533653939E-5,
-101.978374451692));
#22864=CARTESIAN_POINT('Ctrl Pts',(-68.3519492040121,7.51735369854956E-5,
-101.980034593268));
#22865=CARTESIAN_POINT('Ctrl Pts',(-68.3513822292988,8.29462435779145E-5,
-101.981587324641));
#22866=CARTESIAN_POINT('Ctrl Pts',(-68.3508303231258,9.11060791431646E-5,
-101.983098786388));
#22867=CARTESIAN_POINT('Ctrl Pts',(-68.350280785426,9.97858279365715E-5,
-101.984603756704));
#22868=CARTESIAN_POINT('Ctrl Pts',(-68.3497303427571,0.000108479870387661,
-101.986111205378));
#22869=CARTESIAN_POINT('Ctrl Pts',(-68.3491791791713,0.000117743553775951,
-101.987620623011));
#22870=CARTESIAN_POINT('Ctrl Pts',(-68.3486132068006,0.000127862609702767,
-101.989170588042));
#22871=CARTESIAN_POINT('Ctrl Pts',(-68.3480004704559,0.000138817761689317,
-101.990848620322));
#22872=CARTESIAN_POINT('Ctrl Pts',(-68.3473705590191,0.000150785773284043,
-101.992573678939));
#22873=CARTESIAN_POINT('Ctrl Pts',(-68.3467264521374,0.000163820817507876,
-101.994337602245));
#22874=CARTESIAN_POINT('Ctrl Pts',(-68.3459735972113,0.000179056638668035,
-101.996399338252));
#22875=CARTESIAN_POINT('Ctrl Pts',(-68.3452016456489,0.00019576893702528,
-101.998513357157));
#22876=CARTESIAN_POINT('Ctrl Pts',(-68.3444394655154,0.00021337221006501,
-102.000600602695));
#22877=CARTESIAN_POINT('Ctrl Pts',(-68.3435245038817,0.000234504116753176,
-102.003106243427));
#22878=CARTESIAN_POINT('Ctrl Pts',(-68.3426252430714,0.000256914204160928,
-102.005568866458));
#22879=CARTESIAN_POINT('Ctrl Pts',(-68.3418091957487,0.000278444425536151,
-102.007803594829));
#22880=CARTESIAN_POINT('Ctrl Pts',(-68.3411802068165,0.000295039383418406,
-102.009526067744));
#22881=CARTESIAN_POINT('Ctrl Pts',(-68.3406014416822,0.000311061775608003,
-102.011110994502));
#22882=CARTESIAN_POINT('Ctrl Pts',(-68.340096913208,0.000325452808408677,
-102.012492621815));
#22883=CARTESIAN_POINT('Ctrl Pts',(-68.3396386155056,0.000338525167266646,
-102.013747648352));
#22884=CARTESIAN_POINT('Ctrl Pts',(-68.3392418920764,0.000350230045051696,
-102.014834051977));
#22885=CARTESIAN_POINT('Ctrl Pts',(-68.338911958005,0.000360129655326169,
-102.015737555252));
#22886=CARTESIAN_POINT('Ctrl Pts',(-68.338602367729,0.000369418853813961,
-102.01658534835));
#22887=CARTESIAN_POINT('Ctrl Pts',(-68.338351785533,0.00037710798045477,
-102.017271549939));
#22888=CARTESIAN_POINT('Ctrl Pts',(-68.33814917651,0.000383380404201716,
-102.017826380339));
#22889=CARTESIAN_POINT('Ctrl Pts',(-68.3379595836666,0.000389249869614026,
-102.018345566857));
#22890=CARTESIAN_POINT('Ctrl Pts',(-68.3378120837904,0.000393876634263669,
-102.018749484727));
#22891=CARTESIAN_POINT('Ctrl Pts',(-68.3376818644882,0.00039798407021685,
-102.019106081145));
#22892=CARTESIAN_POINT('Ctrl Pts',(-68.3376273573398,0.000399703359268928,
-102.019255345145));
#22893=CARTESIAN_POINT('Ctrl Pts',(-68.3375756725639,0.000401339005957926,
-102.01939688029));
#22894=CARTESIAN_POINT('Ctrl Pts',(-68.3375240385289,0.000402977856687414,
-102.019538276432));
#22895=CARTESIAN_POINT('',(-67.9629492358567,0.0221748193627333,-101.882759497799));
#22896=CARTESIAN_POINT('Ctrl Pts',(-67.9629492358567,0.0221748193627333,
-101.882759497799));
#22897=CARTESIAN_POINT('Ctrl Pts',(-68.0878075034141,0.0149175388607179,
-101.92835242401));
#22898=CARTESIAN_POINT('Ctrl Pts',(-68.2126657709715,0.00766025835870256,
-101.973945350221));
#22899=CARTESIAN_POINT('Ctrl Pts',(-68.3375240385289,0.000402977856687192,
-102.019538276432));
#22900=CARTESIAN_POINT('',(-68.15,4.16333634234434E-16,-101.366904810515));
#22901=CARTESIAN_POINT('Ctrl Pts',(-67.9629492358567,0.0221748193627326,
-101.882759497799));
#22902=CARTESIAN_POINT('Ctrl Pts',(-67.963479204653,0.0220473728994396,
-101.881266741523));
#22903=CARTESIAN_POINT('Ctrl Pts',(-67.9640107571927,0.0219200770074053,
-101.879769844391));
#22904=CARTESIAN_POINT('Ctrl Pts',(-67.9645984647885,0.0217800627449767,
-101.878114792924));
#22905=CARTESIAN_POINT('Ctrl Pts',(-67.9652135065934,0.0216335364361574,
-101.876382765213));
#22906=CARTESIAN_POINT('Ctrl Pts',(-67.9658900396362,0.0214730787737821,
-101.874477552795));
#22907=CARTESIAN_POINT('Ctrl Pts',(-67.9666715313617,0.0212890956287135,
-101.872276993515));
#22908=CARTESIAN_POINT('Ctrl Pts',(-67.9674818862734,0.0210983173512174,
-101.869995159986));
#22909=CARTESIAN_POINT('Ctrl Pts',(-67.9684050288704,0.0208822544197106,
-101.867395949033));
#22910=CARTESIAN_POINT('Ctrl Pts',(-67.9694699998139,0.0206355672518712,
-101.864398540544));
#22911=CARTESIAN_POINT('Ctrl Pts',(-67.9705830508428,0.0203777429350113,
-101.861265808498));
#22912=CARTESIAN_POINT('Ctrl Pts',(-67.9718509454421,0.0200864902186626,
-101.857698345532));
#22913=CARTESIAN_POINT('Ctrl Pts',(-67.9732871132033,0.0197612188310728,
-101.853660121473));
#22914=CARTESIAN_POINT('Ctrl Pts',(-67.9748066016365,0.0194170765069945,
-101.849387615911));
#22915=CARTESIAN_POINT('Ctrl Pts',(-67.9765143547195,0.0190349035407727,
-101.844588446135));
#22916=CARTESIAN_POINT('Ctrl Pts',(-67.9784060294671,0.0186194849647396,
-101.839277485123));
#22917=CARTESIAN_POINT('Ctrl Pts',(-67.980450937861,0.0181704157290355,
-101.833536313833));
#22918=CARTESIAN_POINT('Ctrl Pts',(-67.9827106320596,0.0176825934726907,
-101.827197519925));
#22919=CARTESIAN_POINT('Ctrl Pts',(-67.9851583897371,0.0171671675728304,
-101.820339719563));
#22920=CARTESIAN_POINT('Ctrl Pts',(-67.9879348778888,0.0165825206867542,
-101.812560926087));
#22921=CARTESIAN_POINT('Ctrl Pts',(-67.9909530856542,0.0159625611116039,
-101.80411516068));
#22922=CARTESIAN_POINT('Ctrl Pts',(-67.9941504668417,0.0153275058890211,
-101.795182272282));
#22923=CARTESIAN_POINT('Ctrl Pts',(-67.999103381522,0.0143437713418104,
-101.781344749796));
#22924=CARTESIAN_POINT('Ctrl Pts',(-68.0044847691745,0.013325450983196,
-101.76634326983));
#22925=CARTESIAN_POINT('Ctrl Pts',(-68.0100131590849,0.0123429144795248,
-101.750973409286));
#22926=CARTESIAN_POINT('Ctrl Pts',(-68.0135448047949,0.0117152505693476,
-101.741154835898));
#22927=CARTESIAN_POINT('Ctrl Pts',(-68.0171353174443,0.0111019329412723,
-101.731188757335));
#22928=CARTESIAN_POINT('Ctrl Pts',(-68.0207185807078,0.0105151587105776,
-101.721259398455));
#22929=CARTESIAN_POINT('Ctrl Pts',(-68.0240778900172,0.00996505786930133,
-101.711950624506));
#22930=CARTESIAN_POINT('Ctrl Pts',(-68.0274303123987,0.00943826307777242,
-101.702675497437));
#22931=CARTESIAN_POINT('Ctrl Pts',(-68.030737812301,0.00893961634699059,
-101.693538665169));
#22932=CARTESIAN_POINT('Ctrl Pts',(-68.0336280436274,0.00850387804171688,
-101.685554520158));
#22933=CARTESIAN_POINT('Ctrl Pts',(-68.0364839523172,0.00808954505312252,
-101.677675989526));
#22934=CARTESIAN_POINT('Ctrl Pts',(-68.0392959553743,0.00769663985092728,
-101.669928535905));
#22935=CARTESIAN_POINT('Ctrl Pts',(-68.0419389442863,0.00732735003445809,
-101.662646739406));
#22936=CARTESIAN_POINT('Ctrl Pts',(-68.0445430543738,0.00697694539912664,
-101.655480972348));
#22937=CARTESIAN_POINT('Ctrl Pts',(-68.047116215687,0.00664325368379659,
-101.648408198893));
#22938=CARTESIAN_POINT('Ctrl Pts',(-68.0495855904285,0.00632302117871791,
-101.641620700561));
#22939=CARTESIAN_POINT('Ctrl Pts',(-68.0520263717414,0.00601814482450214,
-101.634919083727));
#22940=CARTESIAN_POINT('Ctrl Pts',(-68.0544620138332,0.0057251777884475,
-101.628237508679));
#22941=CARTESIAN_POINT('Ctrl Pts',(-68.0569473578203,0.00542623244506826,
-101.62141958891));
#22942=CARTESIAN_POINT('Ctrl Pts',(-68.0594301387455,0.00513933042164893,
-101.61461481663));
#22943=CARTESIAN_POINT('Ctrl Pts',(-68.0619414059947,0.00486121713136911,
-101.607736477541));
#22944=CARTESIAN_POINT('Ctrl Pts',(-68.0645328639825,0.00457422302197651,
-101.600638496719));
#22945=CARTESIAN_POINT('Ctrl Pts',(-68.0671545943895,0.00429665256098612,
-101.593462367059));
#22946=CARTESIAN_POINT('Ctrl Pts',(-68.069820349461,0.00402812635154237,
-101.586169212969));
#22947=CARTESIAN_POINT('Ctrl Pts',(-68.0726342429012,0.0037446779029668,
-101.57847077185));
#22948=CARTESIAN_POINT('Ctrl Pts',(-68.0754970824227,0.00347138491776708,
-101.570642253064));
#22949=CARTESIAN_POINT('Ctrl Pts',(-68.0784041665282,0.00321016784256067,
-101.562695470325));
#22950=CARTESIAN_POINT('Ctrl Pts',(-68.0815330051506,0.00292902493645311,
-101.554142501145));
#22951=CARTESIAN_POINT('Ctrl Pts',(-68.0847129375145,0.00266197584741215,
-101.545452989185));
#22952=CARTESIAN_POINT('Ctrl Pts',(-68.0879165455134,0.00241261000501636,
-101.536700792837));
#22953=CARTESIAN_POINT('Ctrl Pts',(-68.0915250570899,0.00213172684783878,
-101.526842407588));
#22954=CARTESIAN_POINT('Ctrl Pts',(-68.0951633311921,0.0018734474831218,
-101.516905259307));
#22955=CARTESIAN_POINT('Ctrl Pts',(-68.0987689579156,0.00164207254706628,
-101.507058343113));
#22956=CARTESIAN_POINT('Ctrl Pts',(-68.1055598239953,0.00120629915025051,
-101.488512582751));
#22957=CARTESIAN_POINT('Ctrl Pts',(-68.1122324839578,0.000869036017442551,
-101.47029331438));
#22958=CARTESIAN_POINT('Ctrl Pts',(-68.1182843604923,0.000628923333716003,
-101.453763491701));
#22959=CARTESIAN_POINT('Ctrl Pts',(-68.1213794941397,0.000506121613892526,
-101.44530958322));
#22960=CARTESIAN_POINT('Ctrl Pts',(-68.1243116528745,0.000407933319930232,
-101.43729923241));
#22961=CARTESIAN_POINT('Ctrl Pts',(-68.1270242533874,0.000329996143664024,
-101.429886130252));
#22962=CARTESIAN_POINT('Ctrl Pts',(-68.1294687572354,0.000259761796076702,
-101.423205693281));
#22963=CARTESIAN_POINT('Ctrl Pts',(-68.1317347258719,0.000205884902874958,
-101.41701091811));
#22964=CARTESIAN_POINT('Ctrl Pts',(-68.1337950754692,0.000164141575941579,
-101.411375522026));
#22965=CARTESIAN_POINT('Ctrl Pts',(-68.1357220174725,0.000125101128567872,
-101.406105017722));
#22966=CARTESIAN_POINT('Ctrl Pts',(-68.1374689566186,9.66253224390965E-5,
-101.401324211194));
#22967=CARTESIAN_POINT('Ctrl Pts',(-68.1390295368681,7.52229498877099E-5,
-101.397050537999));
#22968=CARTESIAN_POINT('Ctrl Pts',(-68.1404811145484,5.53154787336606E-5,
-101.393075370028));
#22969=CARTESIAN_POINT('Ctrl Pts',(-68.1417714173016,4.15083053098491E-5,
-101.389539080716));
#22970=CARTESIAN_POINT('Ctrl Pts',(-68.1429106739615,3.14122065048217E-5,
-101.386413974701));
#22971=CARTESIAN_POINT('Ctrl Pts',(-68.1440153840732,2.16222594001115E-5,
-101.383383633658));
#22972=CARTESIAN_POINT('Ctrl Pts',(-68.144977967085,1.53159278963511E-5,
-101.380740200471));
#22973=CARTESIAN_POINT('Ctrl Pts',(-68.1458238660413,1.09001335344416E-5,
-101.378414522321));
#22974=CARTESIAN_POINT('Ctrl Pts',(-68.1466475415775,6.60035072704163E-6,
-101.376149944285));
#22975=CARTESIAN_POINT('Ctrl Pts',(-68.1473604970042,4.09626589672126E-6,
-101.374186883115));
#22976=CARTESIAN_POINT('Ctrl Pts',(-68.1480031204067,2.49220895143232E-6,
-101.372415415303));
#22977=CARTESIAN_POINT('Ctrl Pts',(-68.1486256515069,9.38304547818374E-7,
-101.370699334311));
#22978=CARTESIAN_POINT('Ctrl Pts',(-68.1491821314358,2.32998681033309E-7,
-101.369163186818));
#22979=CARTESIAN_POINT('Ctrl Pts',(-68.1497262923671,4.68224196081835E-8,
-101.367660612916));
#22980=CARTESIAN_POINT('Ctrl Pts',(-68.1498177332246,1.55373419849379E-8,
-101.367408120246));
#22981=CARTESIAN_POINT('Ctrl Pts',(-68.1499088672424,5.55111512312578E-16,
-101.367156463661));
#22982=CARTESIAN_POINT('Ctrl Pts',(-68.15,5.55111512312578E-16,-101.366904810515));
#22983=CARTESIAN_POINT('',(-68.2564581294845,2.08166817117217E-16,-101.658452405258));
#22984=CARTESIAN_POINT('Ctrl Pts',(-67.9629492358567,0.0221748193627332,
-101.882759497799));
#22985=CARTESIAN_POINT('Ctrl Pts',(-67.6593813619428,0.0951765737395145,
-102.737815214467));
#22986=CARTESIAN_POINT('Ctrl Pts',(-67.3499999997967,0.389138386673958,
-103.711832874224));
#22987=CARTESIAN_POINT('Ctrl Pts',(-67.35,0.800000000395794,-104.521316838008));
#22988=CARTESIAN_POINT('Ctrl Pts',(-68.0878075034141,0.0149175388607178,
-101.92835242401));
#22989=CARTESIAN_POINT('Ctrl Pts',(-67.7813554129666,0.0668886409596893,
-102.783387485583));
#22990=CARTESIAN_POINT('Ctrl Pts',(-67.4526591694531,0.338541460012509,
-103.754441947976));
#22991=CARTESIAN_POINT('Ctrl Pts',(-67.4229730822988,0.743827073473449,
-104.557333470599));
#22992=CARTESIAN_POINT('Ctrl Pts',(-68.2126657709715,0.00766025835870252,
-101.973945350221));
#22993=CARTESIAN_POINT('Ctrl Pts',(-67.9033294639905,0.0386007081798643,
-102.8289597567));
#22994=CARTESIAN_POINT('Ctrl Pts',(-67.5553183391094,0.287944533351058,
-103.797051021729));
#22995=CARTESIAN_POINT('Ctrl Pts',(-67.4959461645976,0.687654146551103,
-104.593350103189));
#22996=CARTESIAN_POINT('Ctrl Pts',(-68.3375240385289,0.000402977856687192,
-102.019538276432));
#22997=CARTESIAN_POINT('Ctrl Pts',(-68.0253035150143,0.0103127754000391,
-102.874532027816));
#22998=CARTESIAN_POINT('Ctrl Pts',(-67.6579775087658,0.237347606689609,
-103.839660095481));
#22999=CARTESIAN_POINT('Ctrl Pts',(-67.5689192468964,0.631481219628758,
-104.629366735779));
#23000=CARTESIAN_POINT('',(-67.5689192468964,0.631481219628695,-104.629366735779));
#23001=CARTESIAN_POINT('Ctrl Pts',(-68.3375240385289,0.000402977856687192,
-102.019538276432));
#23002=CARTESIAN_POINT('Ctrl Pts',(-68.0253035150143,0.0103127754000391,
-102.874532027816));
#23003=CARTESIAN_POINT('Ctrl Pts',(-67.6579775087658,0.237347606689609,
-103.839660095481));
#23004=CARTESIAN_POINT('Ctrl Pts',(-67.5689192468964,0.631481219628758,
-104.629366735779));
#23005=CARTESIAN_POINT('',(-67.35,0.800000000220445,-104.521316838097));
#23006=CARTESIAN_POINT('',(-67.5689192468964,0.631481219628695,-104.629366735779));
#23007=CARTESIAN_POINT('Ctrl Pts',(-67.35,0.800000000395794,-104.521316838008));
#23008=CARTESIAN_POINT('Ctrl Pts',(-67.3499999997967,0.389138386673958,
-103.711832874224));
#23009=CARTESIAN_POINT('Ctrl Pts',(-67.6593813619428,0.0951765737395145,
-102.737815214467));
#23010=CARTESIAN_POINT('Ctrl Pts',(-67.9629492358567,0.0221748193627332,
-101.882759497799));
#23011=CARTESIAN_POINT('Origin',(-67.45,6.00000000000001,-101.95));
#23012=CARTESIAN_POINT('',(-67.55,3.00667409058086,-107.15));
#23013=CARTESIAN_POINT('',(-67.35,3.10645162089483,-106.976666666667));
#23014=CARTESIAN_POINT('',(-67.55,3.00667409058086,-107.15));
#23015=CARTESIAN_POINT('',(-67.35,0.97333333333333,-104.843548379105));
#23016=CARTESIAN_POINT('Origin',(-67.35,6.00000000000001,-101.95));
#23017=CARTESIAN_POINT('',(-67.55,0.800000000000001,-104.943325909419));
#23018=CARTESIAN_POINT('',(-67.35,0.97333333333333,-104.843548379105));
#23019=CARTESIAN_POINT('Origin',(-67.55,6.00000000000001,-101.95));
#23020=CARTESIAN_POINT('Ctrl Pts',(-67.35,0.80000000039573,-104.521316838008));
#23021=CARTESIAN_POINT('Ctrl Pts',(-67.35,0.856168534250959,-104.631980686636));
#23022=CARTESIAN_POINT('Ctrl Pts',(-67.35,0.913326151321769,-104.739304018183));
#23023=CARTESIAN_POINT('Ctrl Pts',(-67.35,0.97333333333333,-104.843548379105));
#23024=CARTESIAN_POINT('Ctrl Pts',(-67.4229730822988,0.743827073473387,
-104.557333470599));
#23025=CARTESIAN_POINT('Ctrl Pts',(-67.4189147231253,0.79923331718401,-104.667096072329));
#23026=CARTESIAN_POINT('Ctrl Pts',(-67.4166666666667,0.856146146238358,
-104.773601644526));
#23027=CARTESIAN_POINT('Ctrl Pts',(-67.4166666666667,0.915555555555552,
-104.876807555876));
#23028=CARTESIAN_POINT('Ctrl Pts',(-67.4959461645976,0.687654146551043,
-104.593350103189));
#23029=CARTESIAN_POINT('Ctrl Pts',(-67.4878294462506,0.742298100117062,
-104.702211458022));
#23030=CARTESIAN_POINT('Ctrl Pts',(-67.4833333333333,0.798966141154948,
-104.80789927087));
#23031=CARTESIAN_POINT('Ctrl Pts',(-67.4833333333333,0.857777777777775,
-104.910066732648));
#23032=CARTESIAN_POINT('Ctrl Pts',(-67.5689192468964,0.6314812196287,-104.629366735779));
#23033=CARTESIAN_POINT('Ctrl Pts',(-67.556744169376,0.685362883050113,-104.737326843716));
#23034=CARTESIAN_POINT('Ctrl Pts',(-67.55,0.741786136071537,-104.842196897214));
#23035=CARTESIAN_POINT('Ctrl Pts',(-67.55,0.799999999999996,-104.943325909419));
#23036=CARTESIAN_POINT('Ctrl Pts',(-67.35,0.97333333333333,-104.843548379105));
#23037=CARTESIAN_POINT('Ctrl Pts',(-67.35,0.913326151321769,-104.739304018183));
#23038=CARTESIAN_POINT('Ctrl Pts',(-67.35,0.856168534250959,-104.631980686636));
#23039=CARTESIAN_POINT('Ctrl Pts',(-67.35,0.80000000039573,-104.521316838008));
#23040=CARTESIAN_POINT('Ctrl Pts',(-67.5689192468964,0.6314812196287,-104.629366735779));
#23041=CARTESIAN_POINT('Ctrl Pts',(-67.556744169376,0.685362883050113,-104.737326843716));
#23042=CARTESIAN_POINT('Ctrl Pts',(-67.55,0.741786136071537,-104.842196897214));
#23043=CARTESIAN_POINT('Ctrl Pts',(-67.55,0.799999999999996,-104.943325909419));
#23044=CARTESIAN_POINT('Ctrl Pts',(-67.35,3.42868316199157,-107.149999999604));
#23045=CARTESIAN_POINT('Ctrl Pts',(-67.3499999999122,3.7782413927739,-107.327421746315));
#23046=CARTESIAN_POINT('Ctrl Pts',(-67.4083761721518,4.15716092828445,-107.487589107692));
#23047=CARTESIAN_POINT('Ctrl Pts',(-67.6167732367314,5.05523993056306,-107.780574427439));
#23048=CARTESIAN_POINT('Ctrl Pts',(-67.7904716797,5.58142525252587,-107.886348035845));
#23049=CARTESIAN_POINT('Ctrl Pts',(-67.9629497348173,6.06724190764723,-107.927825300627));
#23050=CARTESIAN_POINT('Ctrl Pts',(-67.4229730822988,3.39266652940126,-107.206172926527));
#23051=CARTESIAN_POINT('Ctrl Pts',(-67.4358232888358,3.73937765477556,-107.381196742291));
#23052=CARTESIAN_POINT('Ctrl Pts',(-67.5053957022727,4.11610756215676,-107.53590250564));
#23053=CARTESIAN_POINT('Ctrl Pts',(-67.7336142169646,5.0105732143284,-107.812221615036));
#23054=CARTESIAN_POINT('Ctrl Pts',(-67.9137670393935,5.53583525927463,-107.905551823189));
#23055=CARTESIAN_POINT('Ctrl Pts',(-68.0878080075958,6.02164898271821,-107.935082546577));
#23056=CARTESIAN_POINT('Ctrl Pts',(-67.4959461645976,3.35664989681094,-107.262345853449));
#23057=CARTESIAN_POINT('Ctrl Pts',(-67.5215538519502,3.70051482143448,-107.434941903931));
#23058=CARTESIAN_POINT('Ctrl Pts',(-67.6024177035411,4.07505262722886,-107.584215982616));
#23059=CARTESIAN_POINT('Ctrl Pts',(-67.8503982285565,4.96591111071775,-107.843862211275));
#23060=CARTESIAN_POINT('Ctrl Pts',(-68.0368334977355,5.49026758263733,-107.924762872196));
#23061=CARTESIAN_POINT('Ctrl Pts',(-68.2126662803743,5.97605605778919,-107.942339792527));
#23062=CARTESIAN_POINT('Ctrl Pts',(-67.5689192468964,3.32063326422062,-107.318518780371));
#23063=CARTESIAN_POINT('Ctrl Pts',(-67.6073771408738,3.66165108343613,-107.488716899907));
#23064=CARTESIAN_POINT('Ctrl Pts',(-67.699437233662,4.03399926110116,-107.632529380564));
#23065=CARTESIAN_POINT('Ctrl Pts',(-67.9672392087896,4.92124439448309,-107.875509398871));
#23066=CARTESIAN_POINT('Ctrl Pts',(-68.1601288574289,5.44467758938609,-107.943966659541));
#23067=CARTESIAN_POINT('Ctrl Pts',(-68.3375245531529,5.93046313286018,-107.949597038478));
#23068=CARTESIAN_POINT('',(-67.35,3.42868316190273,-107.14999999978));
#23069=CARTESIAN_POINT('Ctrl Pts',(-67.9629497348173,6.06724190764723,-107.927825300627));
#23070=CARTESIAN_POINT('Ctrl Pts',(-67.7904716797,5.58142525252587,-107.886348035845));
#23071=CARTESIAN_POINT('Ctrl Pts',(-67.6167732367314,5.05523993056306,-107.780574427439));
#23072=CARTESIAN_POINT('Ctrl Pts',(-67.4083761721518,4.15716092828445,-107.487589107692));
#23073=CARTESIAN_POINT('Ctrl Pts',(-67.3499999999122,3.7782413927739,-107.327421746315));
#23074=CARTESIAN_POINT('Ctrl Pts',(-67.35,3.42868316199157,-107.149999999604));
#23075=CARTESIAN_POINT('',(-67.5689192468964,3.32063326422074,-107.318518780371));
#23076=CARTESIAN_POINT('',(-67.35,3.42868316190273,-107.14999999978));
#23077=CARTESIAN_POINT('Ctrl Pts',(-67.5689192468964,3.32063326422062,-107.318518780371));
#23078=CARTESIAN_POINT('Ctrl Pts',(-67.6073771408738,3.66165108343613,-107.488716899907));
#23079=CARTESIAN_POINT('Ctrl Pts',(-67.699437233662,4.03399926110116,-107.632529380564));
#23080=CARTESIAN_POINT('Ctrl Pts',(-67.9672392087896,4.92124439448309,-107.875509398871));
#23081=CARTESIAN_POINT('Ctrl Pts',(-68.1601288574289,5.44467758938609,-107.943966659541));
#23082=CARTESIAN_POINT('Ctrl Pts',(-68.3375245531529,5.93046313286018,-107.949597038478));
#23083=CARTESIAN_POINT('Ctrl Pts',(-67.35,3.10645162089483,-106.976666666667));
#23084=CARTESIAN_POINT('Ctrl Pts',(-67.35,3.21069598181732,-107.036673848678));
#23085=CARTESIAN_POINT('Ctrl Pts',(-67.35,3.31801931336452,-107.093831465749));
#23086=CARTESIAN_POINT('Ctrl Pts',(-67.35,3.42868316199169,-107.149999999604));
#23087=CARTESIAN_POINT('Ctrl Pts',(-67.4166666666667,3.07319244412351,-107.034444444444));
#23088=CARTESIAN_POINT('Ctrl Pts',(-67.4166666666667,3.17639835547359,-107.093853853762));
#23089=CARTESIAN_POINT('Ctrl Pts',(-67.4189147231253,3.28290392767118,-107.150766682816));
#23090=CARTESIAN_POINT('Ctrl Pts',(-67.4229730822988,3.39266652940138,-107.206172926527));
#23091=CARTESIAN_POINT('Ctrl Pts',(-67.4833333333333,3.03993326735218,-107.092222222222));
#23092=CARTESIAN_POINT('Ctrl Pts',(-67.4833333333333,3.14210072912986,-107.151033858845));
#23093=CARTESIAN_POINT('Ctrl Pts',(-67.4878294462506,3.24778854197784,-107.207701899883));
#23094=CARTESIAN_POINT('Ctrl Pts',(-67.4959461645976,3.35664989681106,-107.262345853449));
#23095=CARTESIAN_POINT('Ctrl Pts',(-67.55,3.00667409058086,-107.15));
#23096=CARTESIAN_POINT('Ctrl Pts',(-67.55,3.10780310278613,-107.208213863928));
#23097=CARTESIAN_POINT('Ctrl Pts',(-67.556744169376,3.2126731562845,-107.26463711695));
#23098=CARTESIAN_POINT('Ctrl Pts',(-67.5689192468964,3.32063326422074,-107.318518780371));
#23099=CARTESIAN_POINT('Ctrl Pts',(-67.35,3.42868316199169,-107.149999999604));
#23100=CARTESIAN_POINT('Ctrl Pts',(-67.35,3.31801931336452,-107.093831465749));
#23101=CARTESIAN_POINT('Ctrl Pts',(-67.35,3.21069598181732,-107.036673848678));
#23102=CARTESIAN_POINT('Ctrl Pts',(-67.35,3.10645162089483,-106.976666666667));
#23103=CARTESIAN_POINT('Ctrl Pts',(-67.55,3.00667409058086,-107.15));
#23104=CARTESIAN_POINT('Ctrl Pts',(-67.55,3.10780310278613,-107.208213863928));
#23105=CARTESIAN_POINT('Ctrl Pts',(-67.556744169376,3.2126731562845,-107.26463711695));
#23106=CARTESIAN_POINT('Ctrl Pts',(-67.5689192468964,3.32063326422074,-107.318518780371));
#23107=CARTESIAN_POINT('Origin',(-68.15,92.25,-107.15));
#23108=CARTESIAN_POINT('',(-68.15,121.,-107.95));
#23109=CARTESIAN_POINT('',(-68.15,92.25,-107.95));
#23110=CARTESIAN_POINT('',(-67.35,123.993325909419,-107.15));
#23111=CARTESIAN_POINT('Ctrl Pts',(-68.15,121.,-107.95));
#23112=CARTESIAN_POINT('Ctrl Pts',(-67.9725091568851,121.486078692623,-107.95));
#23113=CARTESIAN_POINT('Ctrl Pts',(-67.7780133341431,122.014025751789,-107.887608349819));
#23114=CARTESIAN_POINT('Ctrl Pts',(-67.4681119224052,123.043713064318,-107.61628036626));
#23115=CARTESIAN_POINT('Ctrl Pts',(-67.35,123.544851663295,-107.408159534737));
#23116=CARTESIAN_POINT('Ctrl Pts',(-67.35,123.993325909419,-107.15));
#23117=CARTESIAN_POINT('',(-67.35,92.25,-107.15));
#23118=CARTESIAN_POINT('Origin',(-67.35,121.,-107.95));
#23119=CARTESIAN_POINT('',(-71.099583741031,6.,-107.95));
#23120=CARTESIAN_POINT('',(-67.35,6.,-107.95));
#23121=CARTESIAN_POINT('',(-71.3125,6.58309518948457,-107.95));
#23122=CARTESIAN_POINT('',(-71.2060418705155,6.29154759474228,-107.95));
#23123=CARTESIAN_POINT('',(-71.3125,121.,-107.95));
#23124=CARTESIAN_POINT('',(-71.3125,92.25,-107.95));
#23125=CARTESIAN_POINT('',(-67.35,121.,-107.95));
#23126=CARTESIAN_POINT('Origin',(-67.35,6.00000000000001,-101.95));
#23127=CARTESIAN_POINT('',(-71.099583741031,0.,-101.95));
#23128=CARTESIAN_POINT('',(-67.35,0.,-101.95));
#23129=CARTESIAN_POINT('',(-71.1249754475493,0.000402961545106217,-102.019536869093));
#23130=CARTESIAN_POINT('Ctrl Pts',(-71.1249754475493,0.000402961545105995,
-102.019536869093));
#23131=CARTESIAN_POINT('Ctrl Pts',(-71.124851587799,0.00039903034867228,
-102.019197687954));
#23132=CARTESIAN_POINT('Ctrl Pts',(-71.1247261194153,0.000395071000824783,
-102.01885410149));
#23133=CARTESIAN_POINT('Ctrl Pts',(-71.1245663846202,0.000390082845616924,
-102.018416679127));
#23134=CARTESIAN_POINT('Ctrl Pts',(-71.1243992161203,0.000384862552676827,
-102.017958900093));
#23135=CARTESIAN_POINT('Ctrl Pts',(-71.124194657536,0.00037851896831914,
-102.017398731222));
#23136=CARTESIAN_POINT('Ctrl Pts',(-71.1239352655514,0.000370623381937385,
-102.016688403951));
#23137=CARTESIAN_POINT('Ctrl Pts',(-71.1236418508271,0.000361692183446622,
-102.015884907726));
#23138=CARTESIAN_POINT('Ctrl Pts',(-71.123278284165,0.000350777273635938,
-102.014889304042));
#23139=CARTESIAN_POINT('Ctrl Pts',(-71.1228435347465,0.000338137262748894,
-102.013698766206));
#23140=CARTESIAN_POINT('Ctrl Pts',(-71.1223678613857,0.000324307419154685,
-102.012396160361));
#23141=CARTESIAN_POINT('Ctrl Pts',(-71.1218074193177,0.000308441358892688,
-102.010861414961));
#23142=CARTESIAN_POINT('Ctrl Pts',(-71.1211844502614,0.000291620849225183,
-102.009155432109));
#23143=CARTESIAN_POINT('Ctrl Pts',(-71.1202527752878,0.000266465108755621,
-102.006604066976));
#23144=CARTESIAN_POINT('Ctrl Pts',(-71.1191829299107,0.000239334834657964,
-102.003674304497));
#23145=CARTESIAN_POINT('Ctrl Pts',(-71.1180892999079,0.000214037091799568,
-102.000679377361));
#23146=CARTESIAN_POINT('Ctrl Pts',(-71.1173517759251,0.00019697675876076,
-101.99865965352));
#23147=CARTESIAN_POINT('Ctrl Pts',(-71.1166045457774,0.00018073635052839,
-101.996613335964));
#23148=CARTESIAN_POINT('Ctrl Pts',(-71.1158742950379,0.000165866021002437,
-101.994613504015));
#23149=CARTESIAN_POINT('Ctrl Pts',(-71.1152379645436,0.00015290821948918,
-101.992870877841));
#23150=CARTESIAN_POINT('Ctrl Pts',(-71.1146147686253,0.000140979678841012,
-101.991164211349));
#23151=CARTESIAN_POINT('Ctrl Pts',(-71.1140085827462,0.000130049362750739,
-101.989504119281));
#23152=CARTESIAN_POINT('Ctrl Pts',(-71.1134416133361,0.000119826170360816,
-101.98795142488));
#23153=CARTESIAN_POINT('Ctrl Pts',(-71.1128897131664,0.000110468349252261,
-101.986439991042));
#23154=CARTESIAN_POINT('Ctrl Pts',(-71.1123401816121,0.00010170560401157,
-101.984935038344));
#23155=CARTESIAN_POINT('Ctrl Pts',(-71.1117897479163,9.29284733604459E-5,
-101.983427615032));
#23156=CARTESIAN_POINT('Ctrl Pts',(-71.1112385933679,8.46980842703503E-5,
-101.98191821223));
#23157=CARTESIAN_POINT('Ctrl Pts',(-71.1106726308321,7.68530591930272E-5,
-101.980368253225));
#23158=CARTESIAN_POINT('Ctrl Pts',(-71.1100599017399,6.83597848340904E-5,
-101.978690218171));
#23159=CARTESIAN_POINT('Ctrl Pts',(-71.1094299982868,6.03342636038971E-5,
-101.976965145765));
#23160=CARTESIAN_POINT('Ctrl Pts',(-71.1087859004829,5.29252693262094E-5,
-101.975201198996));
#23161=CARTESIAN_POINT('Ctrl Pts',(-71.1080330497704,4.42653009376351E-5,
-101.973139418046));
#23162=CARTESIAN_POINT('Ctrl Pts',(-71.1072611035879,3.64757776301905E-5,
-101.971025339841));
#23163=CARTESIAN_POINT('Ctrl Pts',(-71.1064989308872,2.98874829738338E-5,
-101.968938027944));
#23164=CARTESIAN_POINT('Ctrl Pts',(-71.1055840060273,2.19787838566663E-5,
-101.966432383826));
#23165=CARTESIAN_POINT('Ctrl Pts',(-71.1046847841119,1.58466565800604E-5,
-101.963969744833));
#23166=CARTESIAN_POINT('Ctrl Pts',(-71.1038687722318,1.14758458700237E-5,
-101.961734991212));
#23167=CARTESIAN_POINT('Ctrl Pts',(-71.1032398031926,8.10689416688974E-6,
-101.960012478498));
#23168=CARTESIAN_POINT('Ctrl Pts',(-71.102661057005,5.75949607614505E-6,
-101.958427509908));
#23169=CARTESIAN_POINT('Ctrl Pts',(-71.1021565448688,4.1369944820957E-6,
-101.957045843929));
#23170=CARTESIAN_POINT('Ctrl Pts',(-71.1016982611712,2.66316268176917E-6,
-101.95579077998));
#23171=CARTESIAN_POINT('Ctrl Pts',(-71.1013015498054,1.77620578348578E-6,
-101.954704342338));
#23172=CARTESIAN_POINT('Ctrl Pts',(-71.1009716248581,1.20384665613926E-6,
-101.953800810232));
#23173=CARTESIAN_POINT('Ctrl Pts',(-71.1006620429046,6.66778882898464E-7,
-101.952952989427));
#23174=CARTESIAN_POINT('Ctrl Pts',(-71.1004114665276,4.02530372668449E-7,
-101.952266765024));
#23175=CARTESIAN_POINT('Ctrl Pts',(-71.1002088602548,2.44220883516277E-7,
-101.951711914293));
#23176=CARTESIAN_POINT('Ctrl Pts',(-71.1000192697177,9.60814371089195E-8,
-101.951192708018));
#23177=CARTESIAN_POINT('Ctrl Pts',(-71.099871769579,4.12488911489826E-8,
-101.950788772905));
#23178=CARTESIAN_POINT('Ctrl Pts',(-71.0997415471677,1.55631951770374E-8,
-101.950432155465));
#23179=CARTESIAN_POINT('Ctrl Pts',(-71.0996870475923,4.8134362897241E-9,
-101.950282906969));
#23180=CARTESIAN_POINT('Ctrl Pts',(-71.0996353689583,0.,-101.950141384051));
#23181=CARTESIAN_POINT('Ctrl Pts',(-71.099583741031,0.,-101.95));
#23182=CARTESIAN_POINT('',(-71.8935807531036,0.631481219628703,-104.629366735779));
#23183=CARTESIAN_POINT('Ctrl Pts',(-71.8935807531036,0.63148121962876,-104.629366735779));
#23184=CARTESIAN_POINT('Ctrl Pts',(-71.8045224423712,0.237347390442852,
-103.839659662198));
#23185=CARTESIAN_POINT('Ctrl Pts',(-71.4371961129181,0.0103125630353027,
-102.874531011475));
#23186=CARTESIAN_POINT('Ctrl Pts',(-71.1249754475488,0.000402961545087344,
-102.019536869091));
#23187=CARTESIAN_POINT('',(-71.9125,0.800000000000001,-104.943325909419));
#23188=CARTESIAN_POINT('Ctrl Pts',(-71.9125,0.800000000000002,-104.943325909419));
#23189=CARTESIAN_POINT('Ctrl Pts',(-71.9125,0.741786136071551,-104.842196897214));
#23190=CARTESIAN_POINT('Ctrl Pts',(-71.905755830624,0.685362883050117,-104.737326843716));
#23191=CARTESIAN_POINT('Ctrl Pts',(-71.8935807531036,0.631481219628707,
-104.629366735779));
#23192=CARTESIAN_POINT('',(-71.9125,3.00667409058086,-107.15));
#23193=CARTESIAN_POINT('Origin',(-71.9125,6.00000000000001,-101.95));
#23194=CARTESIAN_POINT('',(-71.8935807531036,3.32063326422075,-107.318518780371));
#23195=CARTESIAN_POINT('Ctrl Pts',(-71.8935807531036,3.32063326422075,-107.318518780371));
#23196=CARTESIAN_POINT('Ctrl Pts',(-71.905755830624,3.2126731562845,-107.26463711695));
#23197=CARTESIAN_POINT('Ctrl Pts',(-71.9125,3.10780310278613,-107.208213863928));
#23198=CARTESIAN_POINT('Ctrl Pts',(-71.9125,3.00667409058086,-107.15));
#23199=CARTESIAN_POINT('',(-71.124975960152,5.93046172723723,-107.949597022186));
#23200=CARTESIAN_POINT('Ctrl Pts',(-71.124975960152,5.93046172723723,-107.949597022186));
#23201=CARTESIAN_POINT('Ctrl Pts',(-71.4371989024855,5.0754613003514,-107.939687147793));
#23202=CARTESIAN_POINT('Ctrl Pts',(-71.8045224912342,4.11033990451893,-107.71265239331));
#23203=CARTESIAN_POINT('Ctrl Pts',(-71.8935807531036,3.32063326422062,-107.318518780371));
#23204=CARTESIAN_POINT('Ctrl Pts',(-71.099583741031,6.,-107.95));
#23205=CARTESIAN_POINT('Ctrl Pts',(-71.0997076101999,5.99966078194888,-107.95));
#23206=CARTESIAN_POINT('Ctrl Pts',(-71.0998330879657,5.99931715853558,-107.949999977092));
#23207=CARTESIAN_POINT('Ctrl Pts',(-71.0999928315222,5.99887969296171,-107.949999895409));
#23208=CARTESIAN_POINT('Ctrl Pts',(-71.1001600092056,5.99842186866603,-107.949999809925));
#23209=CARTESIAN_POINT('Ctrl Pts',(-71.1003645763045,5.99786164766841,-107.949999661008));
#23210=CARTESIAN_POINT('Ctrl Pts',(-71.100623975913,5.99715125904428,-107.949999323723));
#23211=CARTESIAN_POINT('Ctrl Pts',(-71.1009173990571,5.99634769397783,-107.949998942198));
#23212=CARTESIAN_POINT('Ctrl Pts',(-71.1012809729018,5.99535200993297,-107.949998317815));
#23213=CARTESIAN_POINT('Ctrl Pts',(-71.1017157284528,5.99416138284706,-107.949997159212));
#23214=CARTESIAN_POINT('Ctrl Pts',(-71.1021914073829,5.99285868247456,-107.94999589155));
#23215=CARTESIAN_POINT('Ctrl Pts',(-71.1027518533654,5.99132383326823,-107.94999396957));
#23216=CARTESIAN_POINT('Ctrl Pts',(-71.1033748255994,5.98961774499851,-107.949991017392));
#23217=CARTESIAN_POINT('Ctrl Pts',(-71.1043065151119,5.98706619540861,-107.949986602245));
#23218=CARTESIAN_POINT('Ctrl Pts',(-71.1053763764072,5.9841362381271,-107.949979775947));
#23219=CARTESIAN_POINT('Ctrl Pts',(-71.106470023737,5.98114113876118,-107.949970361873));
#23220=CARTESIAN_POINT('Ctrl Pts',(-71.1072075567092,5.97912130615377,-107.949964013218));
#23221=CARTESIAN_POINT('Ctrl Pts',(-71.1079547963995,5.9770748900843,-107.949956536432));
#23222=CARTESIAN_POINT('Ctrl Pts',(-71.1086850574233,5.97507497391498,-107.949948228366));
#23223=CARTESIAN_POINT('Ctrl Pts',(-71.1093213960554,5.97333227660838,-107.949940988841));
#23224=CARTESIAN_POINT('Ctrl Pts',(-71.1099446007125,5.97162554958123,-107.949933136853));
#23225=CARTESIAN_POINT('Ctrl Pts',(-71.1105507958981,5.96996540809479,-107.94992482647));
#23226=CARTESIAN_POINT('Ctrl Pts',(-71.1111177706135,5.9684126767813,-107.949917053764));
#23227=CARTESIAN_POINT('Ctrl Pts',(-71.1116696767866,5.96690121509207,-107.949908893929));
#23228=CARTESIAN_POINT('Ctrl Pts',(-71.112219214484,5.96539624482729,-107.949900214181));
#23229=CARTESIAN_POINT('Ctrl Pts',(-71.112769657144,5.96388879622165,-107.949891520139));
#23230=CARTESIAN_POINT('Ctrl Pts',(-71.1133208207184,5.96237937864895,-107.949882256457));
#23231=CARTESIAN_POINT('Ctrl Pts',(-71.1138867930719,5.96082941367587,-107.949872137401));
#23232=CARTESIAN_POINT('Ctrl Pts',(-71.1144995294067,5.95915138143476,-107.94986118225));
#23233=CARTESIAN_POINT('Ctrl Pts',(-71.1151294408272,5.95742632285292,-107.949849214239));
#23234=CARTESIAN_POINT('Ctrl Pts',(-71.1157735476843,5.95566239958307,-107.949836179196));
#23235=CARTESIAN_POINT('Ctrl Pts',(-71.1165264025987,5.95360066357222,-107.949820943375));
#23236=CARTESIAN_POINT('Ctrl Pts',(-71.117298354139,5.95148664466337,-107.949804231078));
#23237=CARTESIAN_POINT('Ctrl Pts',(-71.1180605342385,5.94939939913612,-107.949786627805));
#23238=CARTESIAN_POINT('Ctrl Pts',(-71.1189754957585,5.94689375861683,-107.949765495901));
#23239=CARTESIAN_POINT('Ctrl Pts',(-71.1198747564399,5.94443113581304,-107.949743085817));
#23240=CARTESIAN_POINT('Ctrl Pts',(-71.1206908036366,5.94219640766141,-107.949721555598));
#23241=CARTESIAN_POINT('Ctrl Pts',(-71.1213197924908,5.94047393486156,-107.949704960642));
#23242=CARTESIAN_POINT('Ctrl Pts',(-71.1218985575461,5.93888900822262,-107.949688938252));
#23243=CARTESIAN_POINT('Ctrl Pts',(-71.1224030859461,5.93750738102305,-107.949674547221));
#23244=CARTESIAN_POINT('Ctrl Pts',(-71.1228613835834,5.93625235458417,-107.949661474864));
#23245=CARTESIAN_POINT('Ctrl Pts',(-71.123258106951,5.93516595105505,-107.949649769988));
#23246=CARTESIAN_POINT('Ctrl Pts',(-71.1235880409681,5.93426244786692,-107.949639870379));
#23247=CARTESIAN_POINT('Ctrl Pts',(-71.1238976311937,5.93341465484948,-107.949630581182));
#23248=CARTESIAN_POINT('Ctrl Pts',(-71.1241482133456,5.93272845333488,-107.949622892056));
#23249=CARTESIAN_POINT('Ctrl Pts',(-71.1243508223328,5.93217362299574,-107.949616619633));
#23250=CARTESIAN_POINT('Ctrl Pts',(-71.1245404151432,5.93165443653311,-107.949610750169));
#23251=CARTESIAN_POINT('Ctrl Pts',(-71.1246879149935,5.93125051870808,-107.949606123405));
#23252=CARTESIAN_POINT('Ctrl Pts',(-71.1248181342775,5.93089392231776,-107.94960201597));
#23253=CARTESIAN_POINT('Ctrl Pts',(-71.1248726413951,5.93074465839334,-107.949600296682));
#23254=CARTESIAN_POINT('Ctrl Pts',(-71.124924326144,5.93060312331329,-107.949598661036));
#23255=CARTESIAN_POINT('Ctrl Pts',(-71.124975960152,5.93046172723723,-107.949597022186));
#23256=CARTESIAN_POINT('Ctrl Pts',(-67.9629497353525,0.0221746992445629,
38.3827580908684));
#23257=CARTESIAN_POINT('Ctrl Pts',(-67.9731885882307,0.0197124752224134,
38.3539184501918));
#23258=CARTESIAN_POINT('Ctrl Pts',(-68.0649766144896,-0.000362008710208082,
38.0974285502451));
#23259=CARTESIAN_POINT('Ctrl Pts',(-68.142152319925,6.41557585660516E-16,
37.8885753209566));
#23260=CARTESIAN_POINT('Ctrl Pts',(-68.15,5.55111512312588E-16,37.8669048105155));
#23261=CARTESIAN_POINT('Ctrl Pts',(-68.0878080077735,0.014917453342971,
38.4283510167903));
#23262=CARTESIAN_POINT('Ctrl Pts',(-68.0951549181673,0.0138762587036523,
38.4077957764774));
#23263=CARTESIAN_POINT('Ctrl Pts',(-68.1598892716053,-0.00240660968547253,
38.2259097718945));
#23264=CARTESIAN_POINT('Ctrl Pts',(-68.2153859993257,1.16858226445236E-15,
38.0766871386273));
#23265=CARTESIAN_POINT('Ctrl Pts',(-68.220972086323,1.11022302462517E-15,
38.061269873677));
#23266=CARTESIAN_POINT('Ctrl Pts',(-68.2126662801947,0.00766020744137906,
38.4739439427121));
#23267=CARTESIAN_POINT('Ctrl Pts',(-68.2170579360371,0.00742672694733014,
38.4617488613535));
#23268=CARTESIAN_POINT('Ctrl Pts',(-68.2567225636689,0.00233198877221449,
38.3525319855683));
#23269=CARTESIAN_POINT('Ctrl Pts',(-68.2886196787263,1.69564431891977E-15,
38.264798956298));
#23270=CARTESIAN_POINT('Ctrl Pts',(-68.291944172646,1.66533453693774E-15,
38.2556349368385));
#23271=CARTESIAN_POINT('Ctrl Pts',(-68.3375245526157,0.000402961539787139,
38.5195368686339));
#23272=CARTESIAN_POINT('Ctrl Pts',(-68.3389416666765,0.000357983621347725,
38.5156562022828));
#23273=CARTESIAN_POINT('Ctrl Pts',(-68.3515732880386,-7.64792169922838E-6,
38.4810647510841));
#23274=CARTESIAN_POINT('Ctrl Pts',(-68.3618533581269,2.22267096799525E-15,
38.4529107739687));
#23275=CARTESIAN_POINT('Ctrl Pts',(-68.3629162589689,2.22044604925032E-15,
38.45));
#23276=CARTESIAN_POINT('',(-68.15,5.55111512312578E-16,37.8669048105155));
#23277=CARTESIAN_POINT('',(-67.9629497353525,0.0221746992445629,38.3827580908684));
#23278=CARTESIAN_POINT('Ctrl Pts',(-68.15,5.55111512312578E-16,37.8669048105155));
#23279=CARTESIAN_POINT('Ctrl Pts',(-68.1494585269693,5.61123070571811E-16,
37.8684000290838));
#23280=CARTESIAN_POINT('Ctrl Pts',(-68.1489155383042,5.09286916023732E-7,
37.8698993845373));
#23281=CARTESIAN_POINT('Ctrl Pts',(-68.1483145418308,1.77548274582495E-6,
37.8715567710143));
#23282=CARTESIAN_POINT('Ctrl Pts',(-68.1476856008852,3.10055275502112E-6,
37.8732912208225));
#23283=CARTESIAN_POINT('Ctrl Pts',(-68.1469931402788,5.24993589625362E-6,
37.8751987160141));
#23284=CARTESIAN_POINT('Ctrl Pts',(-68.14619231509,9.06159155444897E-6,
37.8774013289947));
#23285=CARTESIAN_POINT('Ctrl Pts',(-68.1453619255287,1.30139635753023E-5,
37.8796852566885));
#23286=CARTESIAN_POINT('Ctrl Pts',(-68.1444150906901,1.87480333346877E-5,
37.8822863058685));
#23287=CARTESIAN_POINT('Ctrl Pts',(-68.1433221007964,2.78719466376698E-5,
37.8852852462417));
#23288=CARTESIAN_POINT('Ctrl Pts',(-68.1421797918381,3.74075589610416E-5,
37.8884195080249));
#23289=CARTESIAN_POINT('Ctrl Pts',(-68.1408779239497,5.06497820057028E-5,
37.8919881465915));
#23290=CARTESIAN_POINT('Ctrl Pts',(-68.1394032022783,7.01856549885083E-5,
37.8960271871082));
#23291=CARTESIAN_POINT('Ctrl Pts',(-68.1378429803325,9.08541637308448E-5,
37.9003003999972));
#23292=CARTESIAN_POINT('Ctrl Pts',(-68.1360893895847,0.000118592482698504,
37.9050998368976));
#23293=CARTESIAN_POINT('Ctrl Pts',(-68.1341478197916,0.000157072680741943,
37.910410677669));
#23294=CARTESIAN_POINT('Ctrl Pts',(-68.1320491213154,0.00019866703047275,
37.9161513177811));
#23295=CARTESIAN_POINT('Ctrl Pts',(-68.1297309455157,0.000252874501729824,
37.9224890449922));
#23296=CARTESIAN_POINT('Ctrl Pts',(-68.1272221199459,0.000324335633352324,
37.929345386396));
#23297=CARTESIAN_POINT('Ctrl Pts',(-68.1243771917707,0.000405370277300168,
37.9371202588592));
#23298=CARTESIAN_POINT('Ctrl Pts',(-68.1212874002126,0.000508732092038107,
37.9455612108248));
#23299=CARTESIAN_POINT('Ctrl Pts',(-68.1180188001475,0.000639503818214204,
37.954488825319));
#23300=CARTESIAN_POINT('Ctrl Pts',(-68.1129443831169,0.000842523539561197,
37.9683487158313));
#23301=CARTESIAN_POINT('Ctrl Pts',(-68.1074407997524,0.00111288779766146,
37.9833766395574));
#23302=CARTESIAN_POINT('Ctrl Pts',(-68.1018027353767,0.00145318003085737,
37.9987733555495));
#23303=CARTESIAN_POINT('Ctrl Pts',(-68.0982065898685,0.00167022976713585,
38.0085938945441));
#23304=CARTESIAN_POINT('Ctrl Pts',(-68.0945567832225,0.00191520573025482,
38.0185616386996));
#23305=CARTESIAN_POINT('Ctrl Pts',(-68.0909213110562,0.00218441447119044,
38.0284923792874));
#23306=CARTESIAN_POINT('Ctrl Pts',(-68.0875130559002,0.00243679766581759,
38.0378024485886));
#23307=CARTESIAN_POINT('Ctrl Pts',(-68.0841178992979,0.00271033441022534,
38.0470786218232));
#23308=CARTESIAN_POINT('Ctrl Pts',(-68.0807745892903,0.00300072615336044,
38.0562162719615));
#23309=CARTESIAN_POINT('Ctrl Pts',(-68.0778535622437,0.00325443942968668,
38.0641997742796));
#23310=CARTESIAN_POINT('Ctrl Pts',(-68.0749721105665,0.00352092683955299,
38.0720775254654));
#23311=CARTESIAN_POINT('Ctrl Pts',(-68.072139890947,0.00379788783359269,
38.0798240881857));
#23312=CARTESIAN_POINT('Ctrl Pts',(-68.0694783416282,0.00405815908513241,
38.0871038409948));
#23313=CARTESIAN_POINT('Ctrl Pts',(-68.0668603494036,0.00432761452089939,
38.094267506083));
#23314=CARTESIAN_POINT('Ctrl Pts',(-68.064277898257,0.00460593334325243,
38.1013380936256));
#23315=CARTESIAN_POINT('Ctrl Pts',(-68.061799078346,0.00487308350380365,
38.1081249454139));
#23316=CARTESIAN_POINT('Ctrl Pts',(-68.059353085522,0.00514834350309127,
38.1148258004088));
#23317=CARTESIAN_POINT('Ctrl Pts',(-68.0569163964528,0.00543380215951972,
38.1215064572704));
#23318=CARTESIAN_POINT('Ctrl Pts',(-68.0544290762057,0.00572519226950153,
38.1283259293509));
#23319=CARTESIAN_POINT('Ctrl Pts',(-68.0519486572191,0.00602751459370135,
38.135132075711));
#23320=CARTESIAN_POINT('Ctrl Pts',(-68.0494441195864,0.00634483879065095,
38.1420116774559));
#23321=CARTESIAN_POINT('Ctrl Pts',(-68.04685973585,0.00667227946593975,
38.1491106048705));
#23322=CARTESIAN_POINT('Ctrl Pts',(-68.0442497456397,0.00701574199235293,
38.1562875546711));
#23323=CARTESIAN_POINT('Ctrl Pts',(-68.0416005051211,0.00737805385543411,
38.1635814236488));
#23324=CARTESIAN_POINT('Ctrl Pts',(-68.0388040401881,0.00776050022555862,
38.1712806297719));
#23325=CARTESIAN_POINT('Ctrl Pts',(-68.0359639630212,0.00816399945284095,
38.1791097962615));
#23326=CARTESIAN_POINT('Ctrl Pts',(-68.0330849699915,0.00858931283554232,
38.1870570968145));
#23327=CARTESIAN_POINT('Ctrl Pts',(-68.0299863526566,0.00904707129720536,
38.1956106580789));
#23328=CARTESIAN_POINT('Ctrl Pts',(-68.0268428324837,0.00953016358578083,
38.2043006122038));
#23329=CARTESIAN_POINT('Ctrl Pts',(-68.02368140321,0.0100356893472873,38.213053049198));
#23330=CARTESIAN_POINT('Ctrl Pts',(-68.0201202624502,0.0106051306469534,
38.2229120899764));
#23331=CARTESIAN_POINT('Ctrl Pts',(-68.0165367020469,0.011203134184015,
38.2328496433373));
#23332=CARTESIAN_POINT('Ctrl Pts',(-68.0129916108277,0.0118193726711993,
38.2426965899744));
#23333=CARTESIAN_POINT('Ctrl Pts',(-68.0063167143977,0.0129796610315748,
38.2612369729688));
#23334=CARTESIAN_POINT('Ctrl Pts',(-67.9997811752937,0.0142069876584006,
38.2794496998821));
#23335=CARTESIAN_POINT('Ctrl Pts',(-67.993867728542,0.0153837155594101,
38.295972224156));
#23336=CARTESIAN_POINT('Ctrl Pts',(-67.9908424151136,0.0159857283735882,
38.3044251310064));
#23337=CARTESIAN_POINT('Ctrl Pts',(-67.9879803331532,0.0165735929941208,
38.3124339979299));
#23338=CARTESIAN_POINT('Ctrl Pts',(-67.9853349522781,0.0171300094787392,
38.3198450639127));
#23339=CARTESIAN_POINT('Ctrl Pts',(-67.9829511074834,0.0176314157424178,
38.3265234334561));
#23340=CARTESIAN_POINT('Ctrl Pts',(-67.9807434377889,0.0181071459725225,
38.3327157261395));
#23341=CARTESIAN_POINT('Ctrl Pts',(-67.9787370295873,0.0185468696297888,
38.3383482354825));
#23342=CARTESIAN_POINT('Ctrl Pts',(-67.9768605599421,0.0189581160025026,
38.3436159735227));
#23343=CARTESIAN_POINT('Ctrl Pts',(-67.9751602612767,0.0193377871914143,
38.3483936722831));
#23344=CARTESIAN_POINT('Ctrl Pts',(-67.9736414104918,0.0196810601384272,
38.3526639575534));
#23345=CARTESIAN_POINT('Ctrl Pts',(-67.9722286448025,0.02000035696892,38.3566359820428));
#23346=CARTESIAN_POINT('Ctrl Pts',(-67.9709729001376,0.0202881343017986,
38.3601688836916));
#23347=CARTESIAN_POINT('Ctrl Pts',(-67.9698637173153,0.02054447230098,38.3632904546014));
#23348=CARTESIAN_POINT('Ctrl Pts',(-67.9687881743821,0.0207930359444191,
38.3663173528415));
#23349=CARTESIAN_POINT('Ctrl Pts',(-67.9678505360297,0.0210120088053539,
38.3689572081709));
#23350=CARTESIAN_POINT('Ctrl Pts',(-67.9670258490686,0.021205765242865,
38.3712793095085));
#23351=CARTESIAN_POINT('Ctrl Pts',(-67.9662228312024,0.0213944306254464,
38.3735403963807));
#23352=CARTESIAN_POINT('Ctrl Pts',(-67.9655269913847,0.0215591701240771,
38.3754999694087));
#23353=CARTESIAN_POINT('Ctrl Pts',(-67.9648991165362,0.0217084974503975,
38.3772681263158));
#23354=CARTESIAN_POINT('Ctrl Pts',(-67.9642908652096,0.0218531577191369,
38.378981021468));
#23355=CARTESIAN_POINT('Ctrl Pts',(-67.9637464446629,0.0219833465228433,
38.3805141447143));
#23356=CARTESIAN_POINT('Ctrl Pts',(-67.9632138930181,0.0221112224498099,
38.3820140692215));
#23357=CARTESIAN_POINT('Ctrl Pts',(-67.9631256471495,0.0221324119858056,
38.3822626125173));
#23358=CARTESIAN_POINT('Ctrl Pts',(-67.9630376888859,0.0221535483104188,
38.3825103533209));
#23359=CARTESIAN_POINT('Ctrl Pts',(-67.9629497353525,0.0221746992445633,
38.3827580908684));
#23360=CARTESIAN_POINT('',(-68.3375245526157,0.000402961539787139,38.5195368686339));
#23361=CARTESIAN_POINT('Ctrl Pts',(-68.3375245526157,0.000402961539787139,
38.5195368686339));
#23362=CARTESIAN_POINT('Ctrl Pts',(-68.2126662801947,0.00766020744137906,
38.4739439427121));
#23363=CARTESIAN_POINT('Ctrl Pts',(-68.0878080077735,0.014917453342971,
38.4283510167903));
#23364=CARTESIAN_POINT('Ctrl Pts',(-67.9629497353525,0.0221746992445629,
38.3827580908684));
#23365=CARTESIAN_POINT('',(-68.3629162589689,2.22044604925031E-15,38.45));
#23366=CARTESIAN_POINT('Ctrl Pts',(-68.3375245526157,0.000402961539786695,
38.5195368686339));
#23367=CARTESIAN_POINT('Ctrl Pts',(-68.3376484123646,0.000399030343394364,
38.519197687496));
#23368=CARTESIAN_POINT('Ctrl Pts',(-68.3377738807469,0.000395070995587234,
38.5188541010336));
#23369=CARTESIAN_POINT('Ctrl Pts',(-68.3379336155403,0.000390082840428185,
38.5184166786719));
#23370=CARTESIAN_POINT('Ctrl Pts',(-68.3381007840383,0.00038486254753915,
38.5179588996392));
#23371=CARTESIAN_POINT('Ctrl Pts',(-68.3383053426202,0.000378518963241221,
38.5173987307702));
#23372=CARTESIAN_POINT('Ctrl Pts',(-68.338564734602,0.000370623376931611,
38.5166884035007));
#23373=CARTESIAN_POINT('Ctrl Pts',(-68.3388581493232,0.000361692178520524,
38.5158849072773));
#23374=CARTESIAN_POINT('Ctrl Pts',(-68.3392217159815,0.000350777268805274,
38.514889303595));
#23375=CARTESIAN_POINT('Ctrl Pts',(-68.3396564653955,0.000338137258031779,
38.5136987657616));
#23376=CARTESIAN_POINT('Ctrl Pts',(-68.3401321387519,0.000324307414550922,
38.5123961599182));
#23377=CARTESIAN_POINT('Ctrl Pts',(-68.3406925808146,0.000308441354420271,
38.5108614145199));
#23378=CARTESIAN_POINT('Ctrl Pts',(-68.3413155498654,0.000291620844902418,
38.5091554316702));
#23379=CARTESIAN_POINT('Ctrl Pts',(-68.3422472248276,0.000266465104742255,
38.5066040665502));
#23380=CARTESIAN_POINT('Ctrl Pts',(-68.3433170701914,0.000239334831008019,
38.5036743040879));
#23381=CARTESIAN_POINT('Ctrl Pts',(-68.3444107001817,0.000214037088507091,
38.5006793769712));
#23382=CARTESIAN_POINT('Ctrl Pts',(-68.3451482241569,0.000196976755690901,
38.4986596531413));
#23383=CARTESIAN_POINT('Ctrl Pts',(-68.3458954542973,0.000180736347680724,
38.4966133355963));
#23384=CARTESIAN_POINT('Ctrl Pts',(-68.3466257050307,0.000165866018364547,
38.4946135036599));
#23385=CARTESIAN_POINT('Ctrl Pts',(-68.3472620355198,0.000152908217028115,
38.4928708774956));
#23386=CARTESIAN_POINT('Ctrl Pts',(-68.3478852314339,0.000140979676548259,
38.4911642110139));
#23387=CARTESIAN_POINT('Ctrl Pts',(-68.3484914173096,0.000130049360615558,
38.4895041189565));
#23388=CARTESIAN_POINT('Ctrl Pts',(-68.3490583867176,0.000119826168353269,
38.4879514245622));
#23389=CARTESIAN_POINT('Ctrl Pts',(-68.3496102868861,0.000110468347365426,
38.4864399907313));
#23390=CARTESIAN_POINT('Ctrl Pts',(-68.35015981844,0.000101705602237878,
38.4849350380393));
#23391=CARTESIAN_POINT('Ctrl Pts',(-68.3507102521346,9.2928471713106E-5,
38.4834276147353));
#23392=CARTESIAN_POINT('Ctrl Pts',(-68.3512614066828,8.4698082740561E-5,
38.4819182119414));
#23393=CARTESIAN_POINT('Ctrl Pts',(-68.3518273692186,7.68530577763826E-5,
38.4803682529445));
#23394=CARTESIAN_POINT('Ctrl Pts',(-68.3524400983118,6.83597835248359E-5,
38.4786902178969));
#23395=CARTESIAN_POINT('Ctrl Pts',(-68.3530700017665,6.03342623984873E-5,
38.4769651454958));
#23396=CARTESIAN_POINT('Ctrl Pts',(-68.3537140995719,5.292526822398E-5,
38.475201198733));
#23397=CARTESIAN_POINT('Ctrl Pts',(-68.3544669502882,4.42652999317775E-5,
38.4731394177847));
#23398=CARTESIAN_POINT('Ctrl Pts',(-68.3552388964745,3.64757767242872E-5,
38.4710253395818));
#23399=CARTESIAN_POINT('Ctrl Pts',(-68.356001069178,2.98874821691442E-5,
38.4689380276888));
#23400=CARTESIAN_POINT('Ctrl Pts',(-68.3569159940322,2.19787832524977E-5,
38.4664323836002));
#23401=CARTESIAN_POINT('Ctrl Pts',(-68.3578152159407,1.58466561415058E-5,
38.4639697446387));
#23402=CARTESIAN_POINT('Ctrl Pts',(-68.3586312278135,1.14758455520558E-5,
38.4617349910484));
#23403=CARTESIAN_POINT('Ctrl Pts',(-68.3592601968496,8.10689392889741E-6,
38.4600124783516));
#23404=CARTESIAN_POINT('Ctrl Pts',(-68.3598389430335,5.75949590045699E-6,
38.4584275097792));
#23405=CARTESIAN_POINT('Ctrl Pts',(-68.3603434551658,4.13699435153347E-6,
38.4570458438162));
#23406=CARTESIAN_POINT('Ctrl Pts',(-68.3608017388602,2.66316259131356E-6,
38.4557907798814));
#23407=CARTESIAN_POINT('Ctrl Pts',(-68.3611984502224,1.7762057194213E-6,
38.454704342253));
#23408=CARTESIAN_POINT('Ctrl Pts',(-68.3615283751663,1.20384661084216E-6,
38.4538008101588));
#23409=CARTESIAN_POINT('Ctrl Pts',(-68.3618379571167,6.66778855064765E-7,
38.4529529893644));
#23410=CARTESIAN_POINT('Ctrl Pts',(-68.3620885334905,4.02530356487505E-7,
38.4522667649716));
#23411=CARTESIAN_POINT('Ctrl Pts',(-68.3622911397606,2.44220873746315E-7,
38.4517119142492));
#23412=CARTESIAN_POINT('Ctrl Pts',(-68.3624807302953,9.6081433271387E-8,
38.4511927079823));
#23413=CARTESIAN_POINT('Ctrl Pts',(-68.3626282304319,4.1248889315617E-8,
38.4507887728746));
#23414=CARTESIAN_POINT('Ctrl Pts',(-68.3627584528418,1.55631951770374E-8,
38.4504321554389));
#23415=CARTESIAN_POINT('Ctrl Pts',(-68.3628129524137,4.81343762933541E-9,
38.4502829069525));
#23416=CARTESIAN_POINT('Ctrl Pts',(-68.3628646310447,1.77646490962825E-15,
38.4501413840425));
#23417=CARTESIAN_POINT('Ctrl Pts',(-68.3629162589689,1.77635683940025E-15,
38.45));
#23418=CARTESIAN_POINT('',(-68.2564581294845,1.38777878078145E-15,38.1584524052577));
#23419=CARTESIAN_POINT('Ctrl Pts',(-68.337524038529,5.93046172356853,44.4495970221433));
#23420=CARTESIAN_POINT('Ctrl Pts',(-68.3380554670654,5.93191700291027,44.4496138895457));
#23421=CARTESIAN_POINT('Ctrl Pts',(-68.33972470056,5.93648800368254,44.4496722893984));
#23422=CARTESIAN_POINT('Ctrl Pts',(-68.3466592038245,5.95547810050877,44.449843145505));
#23423=CARTESIAN_POINT('Ctrl Pts',(-68.3522696681409,5.97084299769377,44.4499400860122));
#23424=CARTESIAN_POINT('Ctrl Pts',(-68.3583197127975,5.98741189639329,44.4499921112246));
#23425=CARTESIAN_POINT('Ctrl Pts',(-68.3618851430649,5.99717624795805,44.4500002303499));
#23426=CARTESIAN_POINT('Ctrl Pts',(-68.3625619515145,5.99902972236498,44.45));
#23427=CARTESIAN_POINT('Ctrl Pts',(-68.3629162589689,6.,44.45));
#23428=CARTESIAN_POINT('Ctrl Pts',(-68.2126657709715,5.97605464977923,44.4423397416413));
#23429=CARTESIAN_POINT('Ctrl Pts',(-68.2143126524885,5.98062783486323,44.4424272990272));
#23430=CARTESIAN_POINT('Ctrl Pts',(-68.2207643044116,5.99843724151488,44.4431085011719));
#23431=CARTESIAN_POINT('Ctrl Pts',(-68.2398084203356,6.05086488453047,44.445030680802));
#23432=CARTESIAN_POINT('Ctrl Pts',(-68.2597610177883,6.1057974519237,44.447239609276));
#23433=CARTESIAN_POINT('Ctrl Pts',(-68.277199866261,6.15377628468129,44.4488972071928));
#23434=CARTESIAN_POINT('Ctrl Pts',(-68.2878612524352,6.18311475992958,44.449788194713));
#23435=CARTESIAN_POINT('Ctrl Pts',(-68.2908360008298,6.19131037030115,44.45));
#23436=CARTESIAN_POINT('Ctrl Pts',(-68.291944172646,6.19436506316151,44.45));
#23437=CARTESIAN_POINT('Ctrl Pts',(-68.0878075034141,6.02164757598992,44.4350824611393));
#23438=CARTESIAN_POINT('Ctrl Pts',(-68.0905626050853,6.02935582072253,44.4354729132527));
#23439=CARTESIAN_POINT('Ctrl Pts',(-68.0980970765099,6.0500556176474,44.4375085746815));
#23440=CARTESIAN_POINT('Ctrl Pts',(-68.1376006723052,6.15744101353435,44.4426124063033));
#23441=CARTESIAN_POINT('Ctrl Pts',(-68.1645086369594,6.23181080403112,44.4468591341426));
#23442=CARTESIAN_POINT('Ctrl Pts',(-68.1976137828852,6.32327377665533,44.4489683068506));
#23443=CARTESIAN_POINT('Ctrl Pts',(-68.216530184342,6.3761496036587,44.4495903553226));
#23444=CARTESIAN_POINT('Ctrl Pts',(-68.219110050145,6.38359101823731,44.45));
#23445=CARTESIAN_POINT('Ctrl Pts',(-68.220972086323,6.38873012632302,44.45));
#23446=CARTESIAN_POINT('Ctrl Pts',(-67.9629492358566,6.06724050220062,44.4278251806373));
#23447=CARTESIAN_POINT('Ctrl Pts',(-67.9667888156612,6.07805539713409,44.4287485196527));
#23448=CARTESIAN_POINT('Ctrl Pts',(-67.9787581135963,6.11198288397358,44.4319313091104));
#23449=CARTESIAN_POINT('Ctrl Pts',(-68.0292786066066,6.25280322257157,44.4413031100688));
#23450=CARTESIAN_POINT('Ctrl Pts',(-68.0708345311172,6.36674803437274,44.4466862872856));
#23451=CARTESIAN_POINT('Ctrl Pts',(-68.1158705867169,6.48963058632797,44.449565613891));
#23452=CARTESIAN_POINT('Ctrl Pts',(-68.1423752254407,6.56208650902341,44.4500126088173));
#23453=CARTESIAN_POINT('Ctrl Pts',(-68.1473840994603,6.57587166617348,44.45));
#23454=CARTESIAN_POINT('Ctrl Pts',(-68.15,6.58309518948453,44.45));
#23455=CARTESIAN_POINT('',(-68.3629162589689,6.,44.45));
#23456=CARTESIAN_POINT('',(-68.337524038529,5.93046172356853,44.4495970221433));
#23457=CARTESIAN_POINT('Ctrl Pts',(-68.3629162589689,6.,44.45));
#23458=CARTESIAN_POINT('Ctrl Pts',(-68.3627923897953,5.99966078193582,44.45));
#23459=CARTESIAN_POINT('Ctrl Pts',(-68.3626669120248,5.99931715850946,44.449999977092));
#23460=CARTESIAN_POINT('Ctrl Pts',(-68.3625071684643,5.99887969292084,44.4499998954093));
#23461=CARTESIAN_POINT('Ctrl Pts',(-68.3623399907767,5.99842186860966,44.4499998099254));
#23462=CARTESIAN_POINT('Ctrl Pts',(-68.3621354236744,5.99786164759464,44.4499996610084));
#23463=CARTESIAN_POINT('Ctrl Pts',(-68.3618760240636,5.99715125894938,44.4499993237228));
#23464=CARTESIAN_POINT('Ctrl Pts',(-68.3615826009174,5.99634769386054,44.449998942198));
#23465=CARTESIAN_POINT('Ctrl Pts',(-68.3612190270722,5.99535200978922,44.4499983178149));
#23466=CARTESIAN_POINT('Ctrl Pts',(-68.3607842715223,5.99416138267066,44.4499971592116));
#23467=CARTESIAN_POINT('Ctrl Pts',(-68.3603085925964,5.99285868227063,44.4499958915495));
#23468=CARTESIAN_POINT('Ctrl Pts',(-68.359748146621,5.99132383303226,44.4499939695697));
#23469=CARTESIAN_POINT('Ctrl Pts',(-68.3591251743955,5.98961774472287,44.4499910173912));
#23470=CARTESIAN_POINT('Ctrl Pts',(-68.3581934848705,5.98706619500446,44.4499866022445));
#23471=CARTESIAN_POINT('Ctrl Pts',(-68.3571236235583,5.98413623755589,44.4499797759452));
#23472=CARTESIAN_POINT('Ctrl Pts',(-68.3560299762101,5.98114113800634,44.4499703618705));
#23473=CARTESIAN_POINT('Ctrl Pts',(-68.3552924432318,5.97912130529265,44.4499640132147));
#23474=CARTESIAN_POINT('Ctrl Pts',(-68.3545452035351,5.97707488911023,44.449956536428));
#23475=CARTESIAN_POINT('Ctrl Pts',(-68.3538149425036,5.97507497282754,44.4499482283617));
#23476=CARTESIAN_POINT('Ctrl Pts',(-68.3531786038672,5.97333227542841,44.4499409888359));
#23477=CARTESIAN_POINT('Ctrl Pts',(-68.3525553992048,5.97162554830819,44.4499331368466));
#23478=CARTESIAN_POINT('Ctrl Pts',(-68.3519492040121,5.96996540673227,44.449924826463));
#23479=CARTESIAN_POINT('Ctrl Pts',(-68.3513822292988,5.96841267535893,44.4499170537564));
#23480=CARTESIAN_POINT('Ctrl Pts',(-68.3508303231258,5.96690121361164,44.4499088939209));
#23481=CARTESIAN_POINT('Ctrl Pts',(-68.350280785426,5.96539624329614,44.4499002141721));
#23482=CARTESIAN_POINT('Ctrl Pts',(-68.3497303427571,5.96388879462198,44.4498915201296));
#23483=CARTESIAN_POINT('Ctrl Pts',(-68.3491791791713,5.96237937698876,44.4498822564462));
#23484=CARTESIAN_POINT('Ctrl Pts',(-68.3486132068006,5.9608294119577,44.4498721373903));
#23485=CARTESIAN_POINT('Ctrl Pts',(-68.3480004704559,5.95915137967762,44.4498611822383));
#23486=CARTESIAN_POINT('Ctrl Pts',(-68.3473705590191,5.95742632106119,44.4498492142267));
#23487=CARTESIAN_POINT('Ctrl Pts',(-68.3467264521375,5.95566239775521,44.4498361791825));
#23488=CARTESIAN_POINT('Ctrl Pts',(-68.3459735972113,5.95360066174812,44.4498209433613));
#23489=CARTESIAN_POINT('Ctrl Pts',(-68.3452016456489,5.95148664284324,44.449804231063));
#23490=CARTESIAN_POINT('Ctrl Pts',(-68.3444394655155,5.94939939730536,44.4497866277899));
#23491=CARTESIAN_POINT('Ctrl Pts',(-68.3435245038817,5.94689375657353,44.4497654958833));
#23492=CARTESIAN_POINT('Ctrl Pts',(-68.3426252430715,5.94443113354186,44.4497430857958));
#23493=CARTESIAN_POINT('Ctrl Pts',(-68.3418091957487,5.94219640517136,44.4497215555745));
#23494=CARTESIAN_POINT('Ctrl Pts',(-68.3411802068166,5.94047393225571,44.4497049606166));
#23495=CARTESIAN_POINT('Ctrl Pts',(-68.3406014416822,5.93888900549839,44.4496889382244));
#23496=CARTESIAN_POINT('Ctrl Pts',(-68.3400969132081,5.93750737818474,44.4496745471916));
#23497=CARTESIAN_POINT('Ctrl Pts',(-68.3396386155056,5.93625235164827,44.4496614748327));
#23498=CARTESIAN_POINT('Ctrl Pts',(-68.3392418920764,5.93516594802355,44.449649769955));
#23499=CARTESIAN_POINT('Ctrl Pts',(-68.338911958005,5.93426244474791,44.4496398703447));
#23500=CARTESIAN_POINT('Ctrl Pts',(-68.338602367729,5.93341465165008,44.4496305811462));
#23501=CARTESIAN_POINT('Ctrl Pts',(-68.338351785533,5.93272845006159,44.4496228920195));
#23502=CARTESIAN_POINT('Ctrl Pts',(-68.33814917651,5.93217361966125,44.4496166195958));
#23503=CARTESIAN_POINT('Ctrl Pts',(-68.3379595836667,5.93165443314326,44.4496107501304));
#23504=CARTESIAN_POINT('Ctrl Pts',(-68.3378120837905,5.93125051527315,44.4496061233657));
#23505=CARTESIAN_POINT('Ctrl Pts',(-68.3376818644882,5.93089391885477,44.4496020159298));
#23506=CARTESIAN_POINT('Ctrl Pts',(-68.3376273573399,5.93074465485525,44.4496002966407));
#23507=CARTESIAN_POINT('Ctrl Pts',(-68.3375756725639,5.93060311970978,44.449598660994));
#23508=CARTESIAN_POINT('Ctrl Pts',(-68.337524038529,5.93046172356853,44.4495970221433));
#23509=CARTESIAN_POINT('',(-67.9629492358566,6.06724050220062,44.4278251806373));
#23510=CARTESIAN_POINT('Ctrl Pts',(-67.9629492358566,6.06724050220062,44.4278251806373));
#23511=CARTESIAN_POINT('Ctrl Pts',(-68.0878075034141,6.02164757598992,44.4350824611393));
#23512=CARTESIAN_POINT('Ctrl Pts',(-68.2126657709715,5.97605464977923,44.4423397416413));
#23513=CARTESIAN_POINT('Ctrl Pts',(-68.337524038529,5.93046172356853,44.4495970221433));
#23514=CARTESIAN_POINT('',(-68.15,6.58309518948453,44.45));
#23515=CARTESIAN_POINT('Ctrl Pts',(-67.9629492358566,6.06724050220062,44.4278251806373));
#23516=CARTESIAN_POINT('Ctrl Pts',(-67.9634792046529,6.06873325847658,44.4279526271005));
#23517=CARTESIAN_POINT('Ctrl Pts',(-67.9640107571925,6.07023015560885,44.4280799229926));
#23518=CARTESIAN_POINT('Ctrl Pts',(-67.9645984647883,6.07188520707584,44.428219937255));
#23519=CARTESIAN_POINT('Ctrl Pts',(-67.9652135065932,6.07361723478624,44.4283664635638));
#23520=CARTESIAN_POINT('Ctrl Pts',(-67.9658900396361,6.07552244720398,44.4285269212262));
#23521=CARTESIAN_POINT('Ctrl Pts',(-67.9666715313615,6.07772300648473,44.4287109043712));
#23522=CARTESIAN_POINT('Ctrl Pts',(-67.9674818862731,6.0800048400133,44.4289016826487));
#23523=CARTESIAN_POINT('Ctrl Pts',(-67.9684050288702,6.08260405096595,44.4291177455802));
#23524=CARTESIAN_POINT('Ctrl Pts',(-67.9694699998137,6.08560145945498,44.4293644327481));
#23525=CARTESIAN_POINT('Ctrl Pts',(-67.9705830508425,6.08873419150098,44.4296222570649));
#23526=CARTESIAN_POINT('Ctrl Pts',(-67.9718509454418,6.0923016544676,44.4299135097813));
#23527=CARTESIAN_POINT('Ctrl Pts',(-67.9732871132029,6.09633987852639,44.4302387811688));
#23528=CARTESIAN_POINT('Ctrl Pts',(-67.9748066016361,6.10061238408877,44.4305829234929));
#23529=CARTESIAN_POINT('Ctrl Pts',(-67.9765143547191,6.10541155386422,44.4309650964591));
#23530=CARTESIAN_POINT('Ctrl Pts',(-67.9784060294667,6.11072251487592,44.4313805150352));
#23531=CARTESIAN_POINT('Ctrl Pts',(-67.9804509378605,6.11646368616668,44.4318295842709));
#23532=CARTESIAN_POINT('Ctrl Pts',(-67.9827106320591,6.1228024800746,44.4323174065272));
#23533=CARTESIAN_POINT('Ctrl Pts',(-67.9851583897365,6.12966028043662,44.4328328324271));
#23534=CARTESIAN_POINT('Ctrl Pts',(-67.9879348778881,6.1374390739121,44.4334174793131));
#23535=CARTESIAN_POINT('Ctrl Pts',(-67.9909530856534,6.1458848393196,44.4340374388882));
#23536=CARTESIAN_POINT('Ctrl Pts',(-67.9941504668408,6.15481772771674,44.4346724941108));
#23537=CARTESIAN_POINT('Ctrl Pts',(-67.9991033815213,6.16865525020394,44.4356562286581));
#23538=CARTESIAN_POINT('Ctrl Pts',(-68.0044847691739,6.18365673017047,44.4366745490167));
#23539=CARTESIAN_POINT('Ctrl Pts',(-68.0100131590845,6.19902659071492,44.4376570855204));
#23540=CARTESIAN_POINT('Ctrl Pts',(-68.0135448047944,6.20884516410302,44.4382847494306));
#23541=CARTESIAN_POINT('Ctrl Pts',(-68.0171353174438,6.21881124266636,44.4388980670586));
#23542=CARTESIAN_POINT('Ctrl Pts',(-68.0207185807072,6.22874060154588,44.4394848412893));
#23543=CARTESIAN_POINT('Ctrl Pts',(-68.0240778900166,6.23804937549544,44.4400349421306));
#23544=CARTESIAN_POINT('Ctrl Pts',(-68.0274303123981,6.24732450256424,44.4405617369221));
#23545=CARTESIAN_POINT('Ctrl Pts',(-68.0307378123003,6.25646133483194,44.4410603836529));
#23546=CARTESIAN_POINT('Ctrl Pts',(-68.0336280436266,6.26444547984301,44.4414961219582));
#23547=CARTESIAN_POINT('Ctrl Pts',(-68.0364839523164,6.27232401047471,44.4419104549468));
#23548=CARTESIAN_POINT('Ctrl Pts',(-68.0392959553735,6.28007146409556,44.442303360149));
#23549=CARTESIAN_POINT('Ctrl Pts',(-68.0419389442854,6.28735326059455,44.4426726499654));
#23550=CARTESIAN_POINT('Ctrl Pts',(-68.044543054373,6.29451902765292,44.4430230546008));
#23551=CARTESIAN_POINT('Ctrl Pts',(-68.0471162156862,6.30159180110784,44.4433567463161));
#23552=CARTESIAN_POINT('Ctrl Pts',(-68.0495855904277,6.30837929944029,44.4436769788212));
#23553=CARTESIAN_POINT('Ctrl Pts',(-68.0520263717406,6.31508091627373,44.4439818551754));
#23554=CARTESIAN_POINT('Ctrl Pts',(-68.0544620138325,6.32176249132158,44.4442748222115));
#23555=CARTESIAN_POINT('Ctrl Pts',(-68.0569473578197,6.32858041109119,44.4445737675549));
#23556=CARTESIAN_POINT('Ctrl Pts',(-68.0594301387449,6.33538518337142,44.4448606695783));
#23557=CARTESIAN_POINT('Ctrl Pts',(-68.0619414059941,6.34226352245981,44.4451387828686));
#23558=CARTESIAN_POINT('Ctrl Pts',(-68.064532863982,6.34936150328192,44.445425776978));
#23559=CARTESIAN_POINT('Ctrl Pts',(-68.0671545943889,6.35653763294209,44.445703347439));
#23560=CARTESIAN_POINT('Ctrl Pts',(-68.0698203494605,6.36383078703253,44.4459718736484));
#23561=CARTESIAN_POINT('Ctrl Pts',(-68.0726342429007,6.37152922815088,44.446255322097));
#23562=CARTESIAN_POINT('Ctrl Pts',(-68.0754970824222,6.37935774693701,44.4465286150822));
#23563=CARTESIAN_POINT('Ctrl Pts',(-68.0784041665278,6.38730452967628,44.4467898321574));
#23564=CARTESIAN_POINT('Ctrl Pts',(-68.0815330051503,6.39585749885638,44.4470709750635));
#23565=CARTESIAN_POINT('Ctrl Pts',(-68.0847129375142,6.40454701081627,44.4473380241526));
#23566=CARTESIAN_POINT('Ctrl Pts',(-68.0879165455132,6.41329920716382,44.447587389995));
#23567=CARTESIAN_POINT('Ctrl Pts',(-68.0915250570896,6.4231575924126,44.4478682731521));
#23568=CARTESIAN_POINT('Ctrl Pts',(-68.0951633311916,6.43309474069371,44.4481265525169));
#23569=CARTESIAN_POINT('Ctrl Pts',(-68.0987689579151,6.44294165688685,44.4483579274529));
#23570=CARTESIAN_POINT('Ctrl Pts',(-68.1055598239949,6.46148741724862,44.4487937008497));
#23571=CARTESIAN_POINT('Ctrl Pts',(-68.1122324839575,6.47970668562001,44.4491309639825));
#23572=CARTESIAN_POINT('Ctrl Pts',(-68.118284360492,6.49623650829922,44.4493710766663));
#23573=CARTESIAN_POINT('Ctrl Pts',(-68.1213794941395,6.50469041678024,44.4494938783861));
#23574=CARTESIAN_POINT('Ctrl Pts',(-68.1243116528742,6.51270076758936,44.4495920666801));
#23575=CARTESIAN_POINT('Ctrl Pts',(-68.1270242533871,6.52011386974791,44.4496700038563));
#23576=CARTESIAN_POINT('Ctrl Pts',(-68.1294687572352,6.52679430671845,44.4497402382039));
#23577=CARTESIAN_POINT('Ctrl Pts',(-68.1317347258717,6.53298908188991,44.4497941150971));
#23578=CARTESIAN_POINT('Ctrl Pts',(-68.133795075469,6.538624477974,44.4498358584241));
#23579=CARTESIAN_POINT('Ctrl Pts',(-68.1357220174723,6.54389498227775,44.4498748988714));
#23580=CARTESIAN_POINT('Ctrl Pts',(-68.1374689566185,6.54867578880567,44.4499033746776));
#23581=CARTESIAN_POINT('Ctrl Pts',(-68.1390295368681,6.55294946200119,44.4499247770501));
#23582=CARTESIAN_POINT('Ctrl Pts',(-68.1404811145484,6.55692462997174,44.4499446845213));
#23583=CARTESIAN_POINT('Ctrl Pts',(-68.1417714173016,6.56046091928347,44.4499584916947));
#23584=CARTESIAN_POINT('Ctrl Pts',(-68.1429106739614,6.56358602529867,44.4499685877935));
#23585=CARTESIAN_POINT('Ctrl Pts',(-68.1440153840732,6.56661636634192,44.4499783777406));
#23586=CARTESIAN_POINT('Ctrl Pts',(-68.144977967085,6.56925979952851,44.4499846840721));
#23587=CARTESIAN_POINT('Ctrl Pts',(-68.1458238660412,6.57158547767846,44.4499890998665));
#23588=CARTESIAN_POINT('Ctrl Pts',(-68.1466475415774,6.57385005571468,44.4499933996493));
#23589=CARTESIAN_POINT('Ctrl Pts',(-68.1473604970041,6.57581311688528,44.4499959037341));
#23590=CARTESIAN_POINT('Ctrl Pts',(-68.1480031204066,6.57758458469693,44.4499975077911));
#23591=CARTESIAN_POINT('Ctrl Pts',(-68.1486256515068,6.57930066568863,44.4499990616955));
#23592=CARTESIAN_POINT('Ctrl Pts',(-68.1491821314357,6.58083681318181,44.4499997670013));
#23593=CARTESIAN_POINT('Ctrl Pts',(-68.149726292367,6.58233938708418,44.4499999531776));
#23594=CARTESIAN_POINT('Ctrl Pts',(-68.1498177332245,6.58259187975336,44.4499999844627));
#23595=CARTESIAN_POINT('Ctrl Pts',(-68.1499088672424,6.58284353633912,44.45));
#23596=CARTESIAN_POINT('Ctrl Pts',(-68.15,6.58309518948453,44.45));
#23597=CARTESIAN_POINT('',(-68.2564581294845,6.29154759474226,44.45));
#23598=CARTESIAN_POINT('Ctrl Pts',(-67.9629492358566,6.06724050220062,44.4278251806372));
#23599=CARTESIAN_POINT('Ctrl Pts',(-67.6593813620821,5.21218478592245,44.3548234262939));
#23600=CARTESIAN_POINT('Ctrl Pts',(-67.3499999997967,4.23816712577606,44.060861613326));
#23601=CARTESIAN_POINT('Ctrl Pts',(-67.35,3.42868316199151,43.6499999996042));
#23602=CARTESIAN_POINT('Ctrl Pts',(-68.0878075034141,6.02164757598992,44.4350824611393));
#23603=CARTESIAN_POINT('Ctrl Pts',(-67.7813554130122,5.16661251454587,44.3831113590611));
#23604=CARTESIAN_POINT('Ctrl Pts',(-67.4526591694531,4.19555805202367,44.1114585399875));
#23605=CARTESIAN_POINT('Ctrl Pts',(-67.4229730822988,3.3926665294012,43.7061729265265));
#23606=CARTESIAN_POINT('Ctrl Pts',(-68.2126657709715,5.97605464977923,44.4423397416413));
#23607=CARTESIAN_POINT('Ctrl Pts',(-67.9033294639424,5.12104024316929,44.4113992918283));
#23608=CARTESIAN_POINT('Ctrl Pts',(-67.5553183391094,4.15294897827129,44.162055466649));
#23609=CARTESIAN_POINT('Ctrl Pts',(-67.4959461645976,3.35664989681088,43.7623458534489));
#23610=CARTESIAN_POINT('Ctrl Pts',(-68.337524038529,5.93046172356853,44.4495970221433));
#23611=CARTESIAN_POINT('Ctrl Pts',(-68.0253035148726,5.07546797179271,44.4396872245955));
#23612=CARTESIAN_POINT('Ctrl Pts',(-67.6579775087658,4.1103399045189,44.2126523933104));
#23613=CARTESIAN_POINT('Ctrl Pts',(-67.5689192468964,3.32063326422057,43.8185187803712));
#23614=CARTESIAN_POINT('',(-67.5689192468964,3.32063326422069,43.8185187803713));
#23615=CARTESIAN_POINT('Ctrl Pts',(-68.337524038529,5.93046172356853,44.4495970221433));
#23616=CARTESIAN_POINT('Ctrl Pts',(-68.0253035148726,5.07546797179271,44.4396872245955));
#23617=CARTESIAN_POINT('Ctrl Pts',(-67.6579775087658,4.1103399045189,44.2126523933104));
#23618=CARTESIAN_POINT('Ctrl Pts',(-67.5689192468964,3.32063326422057,43.8185187803712));
#23619=CARTESIAN_POINT('',(-67.35,3.42868316190267,43.6499999997796));
#23620=CARTESIAN_POINT('',(-67.5689192468964,3.32063326422069,43.8185187803713));
#23621=CARTESIAN_POINT('Ctrl Pts',(-67.35,3.42868316199151,43.6499999996042));
#23622=CARTESIAN_POINT('Ctrl Pts',(-67.3499999997967,4.23816712577606,44.060861613326));
#23623=CARTESIAN_POINT('Ctrl Pts',(-67.6593813620821,5.21218478592245,44.3548234262939));
#23624=CARTESIAN_POINT('Ctrl Pts',(-67.9629492358566,6.06724050220062,44.4278251806372));
#23625=CARTESIAN_POINT('Origin',(-67.45,6.00000000000001,38.45));
#23626=CARTESIAN_POINT('',(-67.55,0.800000000000003,41.4433259094192));
#23627=CARTESIAN_POINT('',(-67.35,0.973333333333333,41.3435483791052));
#23628=CARTESIAN_POINT('',(-67.55,0.800000000000003,41.4433259094192));
#23629=CARTESIAN_POINT('',(-67.35,3.10645162089482,43.4766666666667));
#23630=CARTESIAN_POINT('Origin',(-67.35,6.00000000000001,38.45));
#23631=CARTESIAN_POINT('',(-67.55,3.00667409058085,43.65));
#23632=CARTESIAN_POINT('',(-67.35,3.10645162089482,43.4766666666667));
#23633=CARTESIAN_POINT('Origin',(-67.55,6.00000000000001,38.45));
#23634=CARTESIAN_POINT('Ctrl Pts',(-67.35,3.42868316199163,43.6499999996043));
#23635=CARTESIAN_POINT('Ctrl Pts',(-67.35,3.31801931336448,43.593831465749));
#23636=CARTESIAN_POINT('Ctrl Pts',(-67.35,3.2106959818173,43.5366738486782));
#23637=CARTESIAN_POINT('Ctrl Pts',(-67.35,3.10645162089482,43.4766666666667));
#23638=CARTESIAN_POINT('Ctrl Pts',(-67.4229730822988,3.39266652940132,43.7061729265266));
#23639=CARTESIAN_POINT('Ctrl Pts',(-67.4189147231253,3.28290392767114,43.650766682816));
#23640=CARTESIAN_POINT('Ctrl Pts',(-67.4166666666667,3.17639835547357,43.5938538537616));
#23641=CARTESIAN_POINT('Ctrl Pts',(-67.4166666666667,3.0731924441235,43.5344444444444));
#23642=CARTESIAN_POINT('Ctrl Pts',(-67.4959461645976,3.356649896811,43.7623458534489));
#23643=CARTESIAN_POINT('Ctrl Pts',(-67.4878294462506,3.24778854197779,43.7077018998829));
#23644=CARTESIAN_POINT('Ctrl Pts',(-67.4833333333333,3.14210072912983,43.651033858845));
#23645=CARTESIAN_POINT('Ctrl Pts',(-67.4833333333333,3.03993326735218,43.5922222222222));
#23646=CARTESIAN_POINT('Ctrl Pts',(-67.5689192468964,3.32063326422068,43.8185187803713));
#23647=CARTESIAN_POINT('Ctrl Pts',(-67.556744169376,3.21267315628445,43.7646371169499));
#23648=CARTESIAN_POINT('Ctrl Pts',(-67.55,3.1078031027861,43.7082138639284));
#23649=CARTESIAN_POINT('Ctrl Pts',(-67.55,3.00667409058085,43.65));
#23650=CARTESIAN_POINT('Ctrl Pts',(-67.35,3.10645162089482,43.4766666666667));
#23651=CARTESIAN_POINT('Ctrl Pts',(-67.35,3.2106959818173,43.5366738486782));
#23652=CARTESIAN_POINT('Ctrl Pts',(-67.35,3.31801931336448,43.593831465749));
#23653=CARTESIAN_POINT('Ctrl Pts',(-67.35,3.42868316199163,43.6499999996043));
#23654=CARTESIAN_POINT('Ctrl Pts',(-67.5689192468964,3.32063326422068,43.8185187803713));
#23655=CARTESIAN_POINT('Ctrl Pts',(-67.556744169376,3.21267315628445,43.7646371169499));
#23656=CARTESIAN_POINT('Ctrl Pts',(-67.55,3.1078031027861,43.7082138639284));
#23657=CARTESIAN_POINT('Ctrl Pts',(-67.55,3.00667409058085,43.65));
#23658=CARTESIAN_POINT('Ctrl Pts',(-67.35,0.800000000395797,41.0213168380085));
#23659=CARTESIAN_POINT('Ctrl Pts',(-67.3499999997967,0.389138161249131,
40.2118324300895));
#23660=CARTESIAN_POINT('Ctrl Pts',(-67.6593820111175,0.0951762114108467,
39.2378132607964));
#23661=CARTESIAN_POINT('Ctrl Pts',(-67.9629497353532,0.0221746992443747,
38.3827580908662));
#23662=CARTESIAN_POINT('Ctrl Pts',(-67.4229730822988,0.743827073473452,
41.0573334705988));
#23663=CARTESIAN_POINT('Ctrl Pts',(-67.4526591857407,0.33854123764703,40.254441507459));
#23664=CARTESIAN_POINT('Ctrl Pts',(-67.7813558695995,0.0668883318015427,
39.2833861208106));
#23665=CARTESIAN_POINT('Ctrl Pts',(-68.0878080077738,0.014917453342854,
38.4283510167895));
#23666=CARTESIAN_POINT('Ctrl Pts',(-67.4959461645976,0.687654146551107,
41.0933501031891));
#23667=CARTESIAN_POINT('Ctrl Pts',(-67.5553183716848,0.287944314044929,
40.2970505848284));
#23668=CARTESIAN_POINT('Ctrl Pts',(-67.9033297280813,0.038600452192239,
39.3289589808248));
#23669=CARTESIAN_POINT('Ctrl Pts',(-68.2126662801944,0.00766020744133335,
38.4739439427128));
#23670=CARTESIAN_POINT('Ctrl Pts',(-67.5689192468964,0.631481219628762,
41.1293667357794));
#23671=CARTESIAN_POINT('Ctrl Pts',(-67.6579775576288,0.237347390442828,
40.3396596621978));
#23672=CARTESIAN_POINT('Ctrl Pts',(-68.0253035865633,0.0103125725829351,
39.374531840839));
#23673=CARTESIAN_POINT('Ctrl Pts',(-68.337524552615,0.000402961539812674,
38.5195368686361));
#23674=CARTESIAN_POINT('',(-67.35,0.800000000220445,41.0213168380973));
#23675=CARTESIAN_POINT('Ctrl Pts',(-67.9629497353532,0.0221746992443747,
38.3827580908662));
#23676=CARTESIAN_POINT('Ctrl Pts',(-67.6593820111175,0.0951762114108467,
39.2378132607964));
#23677=CARTESIAN_POINT('Ctrl Pts',(-67.3499999997967,0.389138161249131,
40.2118324300895));
#23678=CARTESIAN_POINT('Ctrl Pts',(-67.35,0.800000000395797,41.0213168380085));
#23679=CARTESIAN_POINT('',(-67.5689192468964,0.631481219628701,41.1293667357793));
#23680=CARTESIAN_POINT('',(-67.35,0.800000000220445,41.0213168380973));
#23681=CARTESIAN_POINT('Ctrl Pts',(-67.5689192468964,0.631481219628762,
41.1293667357794));
#23682=CARTESIAN_POINT('Ctrl Pts',(-67.6579775576288,0.237347390442828,
40.3396596621978));
#23683=CARTESIAN_POINT('Ctrl Pts',(-68.0253035865633,0.0103125725829351,
39.374531840839));
#23684=CARTESIAN_POINT('Ctrl Pts',(-68.337524552615,0.000402961539812674,
38.5195368686361));
#23685=CARTESIAN_POINT('Ctrl Pts',(-67.35,0.973333333333337,41.3435483791052));
#23686=CARTESIAN_POINT('Ctrl Pts',(-67.35,0.913326151321777,41.2393040181827));
#23687=CARTESIAN_POINT('Ctrl Pts',(-67.35,0.856168534250961,41.1319806866355));
#23688=CARTESIAN_POINT('Ctrl Pts',(-67.35,0.800000000395731,41.0213168380083));
#23689=CARTESIAN_POINT('Ctrl Pts',(-67.4166666666667,0.915555555555558,
41.3768075558765));
#23690=CARTESIAN_POINT('Ctrl Pts',(-67.4166666666667,0.856146146238368,
41.2736016445264));
#23691=CARTESIAN_POINT('Ctrl Pts',(-67.4189147231253,0.799233317184012,
41.1670960723288));
#23692=CARTESIAN_POINT('Ctrl Pts',(-67.4229730822988,0.743827073473387,
41.0573334705987));
#23693=CARTESIAN_POINT('Ctrl Pts',(-67.4833333333333,0.85777777777778,41.4100667326478));
#23694=CARTESIAN_POINT('Ctrl Pts',(-67.4833333333333,0.798966141154958,
41.3078992708702));
#23695=CARTESIAN_POINT('Ctrl Pts',(-67.4878294462506,0.742298100117064,
41.2022114580222));
#23696=CARTESIAN_POINT('Ctrl Pts',(-67.4959461645976,0.687654146551043,
41.093350103189));
#23697=CARTESIAN_POINT('Ctrl Pts',(-67.55,0.800000000000002,41.4433259094191));
#23698=CARTESIAN_POINT('Ctrl Pts',(-67.55,0.741786136071548,41.3421968972139));
#23699=CARTESIAN_POINT('Ctrl Pts',(-67.556744169376,0.685362883050115,41.2373268437155));
#23700=CARTESIAN_POINT('Ctrl Pts',(-67.5689192468964,0.6314812196287,41.1293667357793));
#23701=CARTESIAN_POINT('Ctrl Pts',(-67.35,0.800000000395731,41.0213168380083));
#23702=CARTESIAN_POINT('Ctrl Pts',(-67.35,0.856168534250961,41.1319806866355));
#23703=CARTESIAN_POINT('Ctrl Pts',(-67.35,0.913326151321777,41.2393040181827));
#23704=CARTESIAN_POINT('Ctrl Pts',(-67.35,0.973333333333337,41.3435483791052));
#23705=CARTESIAN_POINT('Ctrl Pts',(-67.55,0.800000000000002,41.4433259094191));
#23706=CARTESIAN_POINT('Ctrl Pts',(-67.55,0.741786136071548,41.3421968972139));
#23707=CARTESIAN_POINT('Ctrl Pts',(-67.556744169376,0.685362883050115,41.2373268437155));
#23708=CARTESIAN_POINT('Ctrl Pts',(-67.5689192468964,0.6314812196287,41.1293667357793));
#23709=CARTESIAN_POINT('Origin',(-67.35,6.,44.45));
#23710=CARTESIAN_POINT('',(-68.15,121.,44.45));
#23711=CARTESIAN_POINT('',(-68.15,34.75,44.45));
#23712=CARTESIAN_POINT('',(-71.3125,121.,44.45));
#23713=CARTESIAN_POINT('',(-67.35,121.,44.45));
#23714=CARTESIAN_POINT('',(-71.3125,6.58309518948451,44.45));
#23715=CARTESIAN_POINT('',(-71.3125,34.75,44.45));
#23716=CARTESIAN_POINT('',(-71.099583741031,6.,44.45));
#23717=CARTESIAN_POINT('',(-71.2060418705155,6.29154759474225,44.45));
#23718=CARTESIAN_POINT('',(-67.35,6.,44.45));
#23719=CARTESIAN_POINT('Origin',(-68.15,34.75,43.65));
#23720=CARTESIAN_POINT('',(-67.35,123.993325909419,43.65));
#23721=CARTESIAN_POINT('',(-67.35,34.75,43.65));
#23722=CARTESIAN_POINT('Ctrl Pts',(-67.35,123.993325909419,43.65));
#23723=CARTESIAN_POINT('Ctrl Pts',(-67.35,123.544851663295,43.9081595347366));
#23724=CARTESIAN_POINT('Ctrl Pts',(-67.4681119224052,123.043713064318,44.1162803662604));
#23725=CARTESIAN_POINT('Ctrl Pts',(-67.7780133341431,122.014025751789,44.387608349819));
#23726=CARTESIAN_POINT('Ctrl Pts',(-67.9725091568851,121.486078692623,44.45));
#23727=CARTESIAN_POINT('Ctrl Pts',(-68.15,121.,44.45));
#23728=CARTESIAN_POINT('Origin',(-67.35,63.5,-31.75));
#23729=CARTESIAN_POINT('',(-67.35,126.2,-104.943325909419));
#23730=CARTESIAN_POINT('Origin',(-67.35,121.,-101.95));
#23731=CARTESIAN_POINT('',(-67.35,126.2,41.4433259094192));
#23732=CARTESIAN_POINT('',(-67.35,126.2,3.35000000000001));
#23733=CARTESIAN_POINT('Origin',(-67.35,121.,38.45));
#23734=CARTESIAN_POINT('',(-67.35,0.800000000000001,-66.85));
#23735=CARTESIAN_POINT('Ctrl Pts',(-71.4995502644831,0.0221746992050148,
-101.882758090412));
#23736=CARTESIAN_POINT('Ctrl Pts',(-71.4893114115449,0.0197124751707447,
-101.853918449787));
#23737=CARTESIAN_POINT('Ctrl Pts',(-71.3975368407587,-0.000373182785439377,
-101.597454849766));
#23738=CARTESIAN_POINT('Ctrl Pts',(-71.320347680068,4.16333634234434E-16,
-101.388575320937));
#23739=CARTESIAN_POINT('Ctrl Pts',(-71.3125,4.16333634234434E-16,-101.366904810515));
#23740=CARTESIAN_POINT('Ctrl Pts',(-71.3746919921718,0.0149174533183786,
-101.928351016639));
#23741=CARTESIAN_POINT('Ctrl Pts',(-71.367345081829,0.0138762572832023,
-101.907795776398));
#23742=CARTESIAN_POINT('Ctrl Pts',(-71.3026241804508,-0.00241774122426398,
-101.725936069398));
#23743=CARTESIAN_POINT('Ctrl Pts',(-71.2471140006721,2.77555756156289E-16,
-101.576687138621));
#23744=CARTESIAN_POINT('Ctrl Pts',(-71.241527913677,2.77555756156289E-16,
-101.561269873677));
#23745=CARTESIAN_POINT('Ctrl Pts',(-71.2498337198606,0.00766020743174241,
-101.973943942866));
#23746=CARTESIAN_POINT('Ctrl Pts',(-71.2454420639835,0.00742672674743362,
-101.961748861474));
#23747=CARTESIAN_POINT('Ctrl Pts',(-71.2057787319611,0.00233147861827002,
-101.852535530178));
#23748=CARTESIAN_POINT('Ctrl Pts',(-71.1738803212761,1.38777878078145E-16,
-101.764798956304));
#23749=CARTESIAN_POINT('Ctrl Pts',(-71.170555827354,1.38777878078145E-16,
-101.755634936838));
#23750=CARTESIAN_POINT('Ctrl Pts',(-71.1249754475493,0.000402961545106217,
-102.019536869093));
#23751=CARTESIAN_POINT('Ctrl Pts',(-71.1235583334697,0.000357983626113174,
-102.01565620272));
#23752=CARTESIAN_POINT('Ctrl Pts',(-71.1109280101655,-7.85197747617509E-6,
-101.98106831054));
#23753=CARTESIAN_POINT('Ctrl Pts',(-71.1006466418801,-3.08148791101958E-32,
-101.952910773988));
#23754=CARTESIAN_POINT('Ctrl Pts',(-71.099583741031,-3.08148791101958E-32,
-101.95));
#23755=CARTESIAN_POINT('',(-71.3125,4.16333634234434E-16,-101.366904810515));
#23756=CARTESIAN_POINT('',(-71.4995502644831,0.0221746992050148,-101.882758090412));
#23757=CARTESIAN_POINT('Ctrl Pts',(-71.3125,5.55111512312578E-16,-101.366904810515));
#23758=CARTESIAN_POINT('Ctrl Pts',(-71.3130414730304,5.55111512312578E-16,
-101.368400029083));
#23759=CARTESIAN_POINT('Ctrl Pts',(-71.3135844616951,5.09286916164813E-7,
-101.369899384535));
#23760=CARTESIAN_POINT('Ctrl Pts',(-71.3141854581669,1.77548274082895E-6,
-101.371556771012));
#23761=CARTESIAN_POINT('Ctrl Pts',(-71.3148143991108,3.10055274469816E-6,
-101.373291220819));
#23762=CARTESIAN_POINT('Ctrl Pts',(-71.3155068597142,5.2499358755341E-6,
-101.375198716011));
#23763=CARTESIAN_POINT('Ctrl Pts',(-71.3163076848976,9.0615914953851E-6,
-101.377401328992));
#23764=CARTESIAN_POINT('Ctrl Pts',(-71.3171380744532,1.30139634765649E-5,
-101.379685256687));
#23765=CARTESIAN_POINT('Ctrl Pts',(-71.3180849092836,1.87480331671879E-5,
-101.382286305868));
#23766=CARTESIAN_POINT('Ctrl Pts',(-71.3191778991655,2.78719463189248E-5,
-101.385285246244));
#23767=CARTESIAN_POINT('Ctrl Pts',(-71.3203202081113,3.74075584838786E-5,
-101.388419508031));
#23768=CARTESIAN_POINT('Ctrl Pts',(-71.3216220759832,5.06497812803995E-5,
-101.391988146601));
#23769=CARTESIAN_POINT('Ctrl Pts',(-71.3230967976336,7.01856538209977E-5,
-101.396027187124));
#23770=CARTESIAN_POINT('Ctrl Pts',(-71.3246570195571,9.08541620961374E-5,
-101.400300400019));
#23771=CARTESIAN_POINT('Ctrl Pts',(-71.3264106102773,0.000118592480379773,
-101.405099836927));
#23772=CARTESIAN_POINT('Ctrl Pts',(-71.3283521800371,0.000157072677346992,
-101.410410677708));
#23773=CARTESIAN_POINT('Ctrl Pts',(-71.3304508784775,0.000198667025918302,
-101.416151317832));
#23774=CARTESIAN_POINT('Ctrl Pts',(-71.3327690542346,0.000252874495557993,
-101.422489045056));
#23775=CARTESIAN_POINT('Ctrl Pts',(-71.3352778797553,0.000324335624839467,
-101.429345386476));
#23776=CARTESIAN_POINT('Ctrl Pts',(-71.3381228078755,0.000405370266158498,
-101.437120258959));
#23777=CARTESIAN_POINT('Ctrl Pts',(-71.3412125993701,0.000508732077344889,
-101.445561210948));
#23778=CARTESIAN_POINT('Ctrl Pts',(-71.3444811993641,0.000639503798671726,
-101.454488825469));
#23779=CARTESIAN_POINT('Ctrl Pts',(-71.3495556162887,0.000842523512674709,
-101.468348716034));
#23780=CARTESIAN_POINT('Ctrl Pts',(-71.3550591995291,0.00111288776034773,
-101.483376639822));
#23781=CARTESIAN_POINT('Ctrl Pts',(-71.3606972637692,0.00145317997930938,
-101.498773355879));
#23782=CARTESIAN_POINT('Ctrl Pts',(-71.3642934091842,0.00167022970610506,
-101.508593894897));
#23783=CARTESIAN_POINT('Ctrl Pts',(-71.3679432157324,0.00191520565810608,
-101.518561639076));
#23784=CARTESIAN_POINT('Ctrl Pts',(-71.3715786877994,0.00218441438644557,
-101.528492379687));
#23785=CARTESIAN_POINT('Ctrl Pts',(-71.3749869428623,0.00243679756926383,
-101.53780244901));
#23786=CARTESIAN_POINT('Ctrl Pts',(-71.3783820993703,0.0027103343005662,
-101.547078622267));
#23787=CARTESIAN_POINT('Ctrl Pts',(-71.3817254092859,0.00300072602968982,
-101.556216272426));
#23788=CARTESIAN_POINT('Ctrl Pts',(-71.3846464362529,0.00325443929384036,
-101.564199774765));
#23789=CARTESIAN_POINT('Ctrl Pts',(-71.387527887852,0.00352092669085103,
-101.57207752597));
#23790=CARTESIAN_POINT('Ctrl Pts',(-71.3903601073981,0.00379788767176015,
-101.579824088709));
#23791=CARTESIAN_POINT('Ctrl Pts',(-71.3930216566499,0.00405815891116113,
-101.58710384154));
#23792=CARTESIAN_POINT('Ctrl Pts',(-71.3956396488113,0.00432761433456298,
-101.59426750665));
#23793=CARTESIAN_POINT('Ctrl Pts',(-71.3982220999012,0.00460593314475144,
-101.601338094212));
#23794=CARTESIAN_POINT('Ctrl Pts',(-71.400700919755,0.00487308329334014,
-101.608124946011));
#23795=CARTESIAN_POINT('Ctrl Pts',(-71.4031469125279,0.00514834328083419,
-101.614825801015));
#23796=CARTESIAN_POINT('Ctrl Pts',(-71.4055836015545,0.0054338019260769,
-101.621506457884));
#23797=CARTESIAN_POINT('Ctrl Pts',(-71.4080709217582,0.00572519202464918,
-101.628325929971));
#23798=CARTESIAN_POINT('Ctrl Pts',(-71.4105513407104,0.0060275143380851,
-101.635132076336));
#23799=CARTESIAN_POINT('Ctrl Pts',(-71.4130558783199,0.00634483852537349,
-101.642011678082));
#23800=CARTESIAN_POINT('Ctrl Pts',(-71.4156402620342,0.00667227919094947,
-101.649110605503));
#23801=CARTESIAN_POINT('Ctrl Pts',(-71.4182502522345,0.0070157417088504,
-101.656287555306));
#23802=CARTESIAN_POINT('Ctrl Pts',(-71.4208994927556,0.00737805356504495,
-101.663581424281));
#23803=CARTESIAN_POINT('Ctrl Pts',(-71.4236959576915,0.00776049992794052,
-101.671280630403));
#23804=CARTESIAN_POINT('Ctrl Pts',(-71.4265360348754,0.00816399914981401,
-101.679109796886));
#23805=CARTESIAN_POINT('Ctrl Pts',(-71.4294150279354,0.00858931252928419,
-101.687057097427));
#23806=CARTESIAN_POINT('Ctrl Pts',(-71.4325136453033,0.00904707098752052,
-101.695610658679));
#23807=CARTESIAN_POINT('Ctrl Pts',(-71.4356571655244,0.0095301632752057,
-101.704300612786));
#23808=CARTESIAN_POINT('Ctrl Pts',(-71.4388185948592,0.0100356890385436,
-101.713053049757));
#23809=CARTESIAN_POINT('Ctrl Pts',(-71.4423797356898,0.0106051303406133,
-101.722912090516));
#23810=CARTESIAN_POINT('Ctrl Pts',(-71.4459632961801,0.0112031338835822,
-101.73284964385));
#23811=CARTESIAN_POINT('Ctrl Pts',(-71.4495083874965,0.0118193723798979,
-101.742696590454));
#23812=CARTESIAN_POINT('Ctrl Pts',(-71.4561832840946,0.0129796607548892,
-101.761236973346));
#23813=CARTESIAN_POINT('Ctrl Pts',(-71.4627188234037,0.0142069874078384,
-101.779449700138));
#23814=CARTESIAN_POINT('Ctrl Pts',(-71.4686322703542,0.015383715339768,
-101.795972224294));
#23815=CARTESIAN_POINT('Ctrl Pts',(-71.4716575838855,0.0159857281699938,
-101.804425131087));
#23816=CARTESIAN_POINT('Ctrl Pts',(-71.474519665947,0.0165735928077044,
-101.812433997953));
#23817=CARTESIAN_POINT('Ctrl Pts',(-71.4771650469162,0.0171300093092834,
-101.819845063882));
#23818=CARTESIAN_POINT('Ctrl Pts',(-71.4795488917966,0.017631415588415,
-101.82652343338));
#23819=CARTESIAN_POINT('Ctrl Pts',(-71.481756561571,0.0181071458337637,
-101.832715726019));
#23820=CARTESIAN_POINT('Ctrl Pts',(-71.4837629698439,0.0185468695051121,
-101.838348235322));
#23821=CARTESIAN_POINT('Ctrl Pts',(-71.4856394395559,0.0189581158910569,
-101.843615973325));
#23822=CARTESIAN_POINT('Ctrl Pts',(-71.4873397382806,0.0193377870921649,
-101.848393672052));
#23823=CARTESIAN_POINT('Ctrl Pts',(-71.4888585891159,0.0196810600497634,
-101.852663957293));
#23824=CARTESIAN_POINT('Ctrl Pts',(-71.4902713548522,0.0200003568901358,
-101.856635981755));
#23825=CARTESIAN_POINT('Ctrl Pts',(-71.4915270995564,0.0202881342314904,
-101.86016888338));
#23826=CARTESIAN_POINT('Ctrl Pts',(-71.4926362824102,0.020544472237551,
-101.863290454269));
#23827=CARTESIAN_POINT('Ctrl Pts',(-71.493711825374,0.0207930358876558,
-101.86631735249));
#23828=CARTESIAN_POINT('Ctrl Pts',(-71.4946494637497,0.0210120087537537,
-101.868957207802));
#23829=CARTESIAN_POINT('Ctrl Pts',(-71.4954741507279,0.0212057651950597,
-101.871279309127));
#23830=CARTESIAN_POINT('Ctrl Pts',(-71.4962771686109,0.0213944305813664,
-101.873540395987));
#23831=CARTESIAN_POINT('Ctrl Pts',(-71.4969730084395,0.0215591700824165,
-101.875499969006));
#23832=CARTESIAN_POINT('Ctrl Pts',(-71.4976008832952,0.0217084974103041,
-101.877268125906));
#23833=CARTESIAN_POINT('Ctrl Pts',(-71.4982091346288,0.0218531576805589,
-101.878981021051));
#23834=CARTESIAN_POINT('Ctrl Pts',(-71.498753555179,0.0219833464849813,
-101.880514144293));
#23835=CARTESIAN_POINT('Ctrl Pts',(-71.499286106827,0.0221112224125953,
-101.882014068798));
#23836=CARTESIAN_POINT('Ctrl Pts',(-71.4993743526924,0.0221324119478113,
-101.882262612083));
#23837=CARTESIAN_POINT('Ctrl Pts',(-71.4994623109528,0.0221535482716482,
-101.882510352875));
#23838=CARTESIAN_POINT('Ctrl Pts',(-71.4995502644831,0.0221746992050154,
-101.882758090412));
#23839=CARTESIAN_POINT('Ctrl Pts',(-71.1249754475493,0.000402961545106217,
-102.019536869093));
#23840=CARTESIAN_POINT('Ctrl Pts',(-71.2498337198606,0.00766020743174241,
-101.973943942866));
#23841=CARTESIAN_POINT('Ctrl Pts',(-71.3746919921718,0.0149174533183786,
-101.928351016639));
#23842=CARTESIAN_POINT('Ctrl Pts',(-71.4995502644831,0.0221746992050148,
-101.882758090412));
#23843=CARTESIAN_POINT('',(-71.2060418705155,2.08166817117217E-16,-101.658452405258));
#23844=CARTESIAN_POINT('Ctrl Pts',(-71.124975960152,5.93046172723723,-107.949597022186));
#23845=CARTESIAN_POINT('Ctrl Pts',(-71.124444531672,5.93191700651268,-107.949613889587));
#23846=CARTESIAN_POINT('Ctrl Pts',(-71.1227720449596,5.93649691589196,-107.949672423109));
#23847=CARTESIAN_POINT('Ctrl Pts',(-71.115838041679,5.95548564468742,-107.949843257531));
#23848=CARTESIAN_POINT('Ctrl Pts',(-71.1102273169597,5.9708512545232,-107.949940211793));
#23849=CARTESIAN_POINT('Ctrl Pts',(-71.1041792426941,5.98741475677251,-107.949992161925));
#23850=CARTESIAN_POINT('Ctrl Pts',(-71.1006141582992,5.99717816092017,-107.950000273964));
#23851=CARTESIAN_POINT('Ctrl Pts',(-71.0999380484668,5.99902972241609,-107.95));
#23852=CARTESIAN_POINT('Ctrl Pts',(-71.099583741031,6.,-107.95));
#23853=CARTESIAN_POINT('Ctrl Pts',(-71.2498342285872,5.97605465101008,-107.942339741564));
#23854=CARTESIAN_POINT('Ctrl Pts',(-71.2481873471739,5.98062783599466,-107.942427298381));
#23855=CARTESIAN_POINT('Ctrl Pts',(-71.2417324406356,5.99844615137056,-107.943108609764));
#23856=CARTESIAN_POINT('Ctrl Pts',(-71.222688824581,6.05087242688524,-107.945030768774));
#23857=CARTESIAN_POINT('Ctrl Pts',(-71.202735966263,6.10580570763075,-107.947239708195));
#23858=CARTESIAN_POINT('Ctrl Pts',(-71.1852990888268,6.15377914453737,-107.948897246887));
#23859=CARTESIAN_POINT('Ctrl Pts',(-71.1746380484977,6.18311667273553,-107.949788229765));
#23860=CARTESIAN_POINT('Ctrl Pts',(-71.1716639991639,6.19131037031831,-107.95));
#23861=CARTESIAN_POINT('Ctrl Pts',(-71.170555827354,6.19436506316152,-107.95));
#23862=CARTESIAN_POINT('Ctrl Pts',(-71.3746924970224,6.02164757478294,-107.935082460943));
#23863=CARTESIAN_POINT('Ctrl Pts',(-71.3719373951989,6.02935581973102,-107.935472908878));
#23864=CARTESIAN_POINT('Ctrl Pts',(-71.3643778675314,6.05012165429468,-107.937512017716));
#23865=CARTESIAN_POINT('Ctrl Pts',(-71.3248781549867,6.157496923129,-107.942615263001));
#23866=CARTESIAN_POINT('Ctrl Pts',(-71.2979681803164,6.23187200229262,-107.946862365475));
#23867=CARTESIAN_POINT('Ctrl Pts',(-71.2648781488486,6.32329497724259,-107.948969720755));
#23868=CARTESIAN_POINT('Ctrl Pts',(-71.2459643513634,6.37616378464998,-107.949591702617));
#23869=CARTESIAN_POINT('Ctrl Pts',(-71.243389949861,6.38359101822054,-107.95));
#23870=CARTESIAN_POINT('Ctrl Pts',(-71.241527913677,6.38873012632304,-107.95));
#23871=CARTESIAN_POINT('Ctrl Pts',(-71.4995507654576,6.06724049855579,-107.927825180321));
#23872=CARTESIAN_POINT('Ctrl Pts',(-71.4957111858325,6.07805539364223,-107.9287485193));
#23873=CARTESIAN_POINT('Ctrl Pts',(-71.48371889734,6.1120489170111,-107.931938553361));
#23874=CARTESIAN_POINT('Ctrl Pts',(-71.4332019511036,6.25285912913773,-107.941309176545));
#23875=CARTESIAN_POINT('Ctrl Pts',(-71.3916442015717,6.36680923016425,-107.94669310563));
#23876=CARTESIAN_POINT('Ctrl Pts',(-71.3466221207365,6.48965178583955,-107.949568361152));
#23877=CARTESIAN_POINT('Ctrl Pts',(-71.3201199739812,6.56210068942826,-107.950014973511));
#23878=CARTESIAN_POINT('Ctrl Pts',(-71.3151159005581,6.57587166612277,-107.95));
#23879=CARTESIAN_POINT('Ctrl Pts',(-71.3125,6.58309518948457,-107.95));
#23880=CARTESIAN_POINT('',(-71.4995507654576,6.06724049855579,-107.927825180321));
#23881=CARTESIAN_POINT('Ctrl Pts',(-71.4995507654576,6.06724049855579,-107.927825180321));
#23882=CARTESIAN_POINT('Ctrl Pts',(-71.3746924970224,6.02164757478294,-107.935082460943));
#23883=CARTESIAN_POINT('Ctrl Pts',(-71.2498342285872,5.97605465101008,-107.942339741564));
#23884=CARTESIAN_POINT('Ctrl Pts',(-71.124975960152,5.93046172723723,-107.949597022186));
#23885=CARTESIAN_POINT('Ctrl Pts',(-71.4995507654576,6.0672404985558,-107.927825180321));
#23886=CARTESIAN_POINT('Ctrl Pts',(-71.4990207966871,6.06873325484982,-107.927952626779));
#23887=CARTESIAN_POINT('Ctrl Pts',(-71.4984892441742,6.07023015200047,-107.928079922666));
#23888=CARTESIAN_POINT('Ctrl Pts',(-71.497901536632,6.07188520349622,-107.928219936917));
#23889=CARTESIAN_POINT('Ctrl Pts',(-71.4972864948831,6.0736172312366,-107.928366463213));
#23890=CARTESIAN_POINT('Ctrl Pts',(-71.4966099619257,6.07552244369565,-107.928526920857));
#23891=CARTESIAN_POINT('Ctrl Pts',(-71.4958284703338,6.07772300303647,-107.928710903972));
#23892=CARTESIAN_POINT('Ctrl Pts',(-71.4950181155607,6.08000483662722,-107.928901682219));
#23893=CARTESIAN_POINT('Ctrl Pts',(-71.494094973154,6.08260404766213,-107.929117745108));
#23894=CARTESIAN_POINT('Ctrl Pts',(-71.4930300024624,6.08560145625756,-107.929364432221));
#23895=CARTESIAN_POINT('Ctrl Pts',(-71.491916951697,6.08873418841456,-107.92962225648));
#23896=CARTESIAN_POINT('Ctrl Pts',(-71.4906490574284,6.09230165151849,-107.929913509125));
#23897=CARTESIAN_POINT('Ctrl Pts',(-71.4892128900655,6.09633987574117,-107.930238780429));
#23898=CARTESIAN_POINT('Ctrl Pts',(-71.4876934020539,6.10061238147606,-107.930582922664));
#23899=CARTESIAN_POINT('Ctrl Pts',(-71.485985649468,6.10541155145357,-107.930965095528));
#23900=CARTESIAN_POINT('Ctrl Pts',(-71.4840939752819,6.11072251269302,-107.931380513992));
#23901=CARTESIAN_POINT('Ctrl Pts',(-71.4820490674957,6.11646368422841,-107.931829583108));
#23902=CARTESIAN_POINT('Ctrl Pts',(-71.4797893739799,6.12280247841059,-107.932317405233));
#23903=CARTESIAN_POINT('Ctrl Pts',(-71.4773416170346,6.12966027906724,-107.932832831001));
#23904=CARTESIAN_POINT('Ctrl Pts',(-71.474565129715,6.13743907287268,-107.933417477737));
#23905=CARTESIAN_POINT('Ctrl Pts',(-71.4715469228454,6.14588483863557,-107.93403743716));
#23906=CARTESIAN_POINT('Ctrl Pts',(-71.4683495425667,6.15481772739554,-107.934672492242));
#23907=CARTESIAN_POINT('Ctrl Pts',(-71.4633966290024,6.16865525125939,-107.93565622663));
#23908=CARTESIAN_POINT('Ctrl Pts',(-71.4580152424454,6.18365673275706,-107.936674546861));
#23909=CARTESIAN_POINT('Ctrl Pts',(-71.4524868534505,6.19902659477151,-107.937657083293));
#23910=CARTESIAN_POINT('Ctrl Pts',(-71.448955208538,6.20884516850782,-107.938284747119));
#23911=CARTESIAN_POINT('Ctrl Pts',(-71.4453646966192,6.21881124737631,-107.938898064687));
#23912=CARTESIAN_POINT('Ctrl Pts',(-71.4417814339702,6.22874060650452,-107.939484838886));
#23913=CARTESIAN_POINT('Ctrl Pts',(-71.4384221252368,6.23804938068721,-107.940034939697));
#23914=CARTESIAN_POINT('Ctrl Pts',(-71.4350697033288,6.24732450793948,-107.940561734482));
#23915=CARTESIAN_POINT('Ctrl Pts',(-71.4317622037675,6.25646134033559,-107.94106038123));
#23916=CARTESIAN_POINT('Ctrl Pts',(-71.4288719727465,6.26444548543854,-107.94149611955));
#23917=CARTESIAN_POINT('Ctrl Pts',(-71.4260160642607,6.27232401612069,-107.94191045257));
#23918=CARTESIAN_POINT('Ctrl Pts',(-71.4232040612964,6.2800714697516,-107.94230335782));
#23919=CARTESIAN_POINT('Ctrl Pts',(-71.4205610724397,6.287353266348,-107.942672647685));
#23920=CARTESIAN_POINT('Ctrl Pts',(-71.41795696231,6.29451903346519,-107.943023052383));
#23921=CARTESIAN_POINT('Ctrl Pts',(-71.4153838008589,6.30159180694595,-107.94335674417));
#23922=CARTESIAN_POINT('Ctrl Pts',(-71.4129144260191,6.30837930520969,-107.943676976741));
#23923=CARTESIAN_POINT('Ctrl Pts',(-71.4104736445188,6.31508092194651,-107.94398185317));
#23924=CARTESIAN_POINT('Ctrl Pts',(-71.4080380021628,6.32176249687741,-107.944274820287));
#23925=CARTESIAN_POINT('Ctrl Pts',(-71.4055526579071,6.32858041652497,-107.944573765714));
#23926=CARTESIAN_POINT('Ctrl Pts',(-71.4030698766341,6.33538518866313,-107.944860667827));
#23927=CARTESIAN_POINT('Ctrl Pts',(-71.4005586089811,6.34226352759248,-107.94513878121));
#23928=CARTESIAN_POINT('Ctrl Pts',(-71.3979671505498,6.34936150832369,-107.945425775418));
#23929=CARTESIAN_POINT('Ctrl Pts',(-71.3953454196391,6.35653763787639,-107.94570334598));
#23930=CARTESIAN_POINT('Ctrl Pts',(-71.392679664026,6.36383079184782,-107.94597187229));
#23931=CARTESIAN_POINT('Ctrl Pts',(-71.389865770012,6.37152923284606,-107.946255320844));
#23932=CARTESIAN_POINT('Ctrl Pts',(-71.3870029298745,6.37935775149941,-107.946528613934));
#23933=CARTESIAN_POINT('Ctrl Pts',(-71.3840958451337,6.38730453409799,-107.94678983111));
#23934=CARTESIAN_POINT('Ctrl Pts',(-71.3809670058234,6.39585750313803,-107.947070974124));
#23935=CARTESIAN_POINT('Ctrl Pts',(-71.3777870727492,6.40454701494908,-107.947338023315));
#23936=CARTESIAN_POINT('Ctrl Pts',(-71.3745834640428,6.41329921114333,-107.947587389251));
#23937=CARTESIAN_POINT('Ctrl Pts',(-71.3709749516525,6.4231575962656,-107.947868272515));
#23938=CARTESIAN_POINT('Ctrl Pts',(-71.3673366767398,6.43309474441533,-107.948126551975));
#23939=CARTESIAN_POINT('Ctrl Pts',(-71.3637310492388,6.44294166047392,-107.948357926994));
#23940=CARTESIAN_POINT('Ctrl Pts',(-71.3569401818035,6.46148742028461,-107.948793700539));
#23941=CARTESIAN_POINT('Ctrl Pts',(-71.3502675206052,6.4797066881043,-107.949130963775));
#23942=CARTESIAN_POINT('Ctrl Pts',(-71.3442156430593,6.4962365102952,-107.949371076525));
#23943=CARTESIAN_POINT('Ctrl Pts',(-71.3411205088944,6.50469041852693,-107.949493878279));
#23944=CARTESIAN_POINT('Ctrl Pts',(-71.3381883496994,6.51270076910323,-107.949592066599));
#23945=CARTESIAN_POINT('Ctrl Pts',(-71.3354757487876,6.52011387105198,-107.949670003794));
#23946=CARTESIAN_POINT('Ctrl Pts',(-71.3330312445731,6.52679430785273,-107.949740238159));
#23947=CARTESIAN_POINT('Ctrl Pts',(-71.3307652756209,6.53298908287031,-107.949794115064));
#23948=CARTESIAN_POINT('Ctrl Pts',(-71.328704925758,6.53862447881893,-107.949835858399));
#23949=CARTESIAN_POINT('Ctrl Pts',(-71.3267779835042,6.54389498300138,-107.949874898855));
#23950=CARTESIAN_POINT('Ctrl Pts',(-71.3250310441515,6.54867578942307,-107.949903374666));
#23951=CARTESIAN_POINT('Ctrl Pts',(-71.3234704637356,6.55294946252823,-107.949924777042));
#23952=CARTESIAN_POINT('Ctrl Pts',(-71.3220188858989,6.55692463041912,-107.949944684516));
#23953=CARTESIAN_POINT('Ctrl Pts',(-71.3207285830242,6.56046091966393,-107.949958491691));
#23954=CARTESIAN_POINT('Ctrl Pts',(-71.3195893262722,6.5635860256247,-107.949968587791));
#23955=CARTESIAN_POINT('Ctrl Pts',(-71.3184846160707,6.56661636661592,-107.94997837774));
#23956=CARTESIAN_POINT('Ctrl Pts',(-71.3175220329967,6.56925979976205,-107.949984684072));
#23957=CARTESIAN_POINT('Ctrl Pts',(-71.3166761339984,6.57158547788221,-107.949989099866));
#23958=CARTESIAN_POINT('Ctrl Pts',(-71.3158524584211,6.5738500558898,-107.949993399649));
#23959=CARTESIAN_POINT('Ctrl Pts',(-71.3151395029723,6.57581311704178,-107.949995903734));
#23960=CARTESIAN_POINT('Ctrl Pts',(-71.3144968795581,6.57758458484338,-107.949997507791));
#23961=CARTESIAN_POINT('Ctrl Pts',(-71.3138743484462,6.5793006658261,-107.949999061696));
#23962=CARTESIAN_POINT('Ctrl Pts',(-71.3133178685153,6.58083681331819,-107.949999767001));
#23963=CARTESIAN_POINT('Ctrl Pts',(-71.3127737075818,6.58233938722563,-107.949999953178));
#23964=CARTESIAN_POINT('Ctrl Pts',(-71.3126822667415,6.58259187984734,-107.949999984463));
#23965=CARTESIAN_POINT('Ctrl Pts',(-71.3125911327406,6.58284353638613,-107.95));
#23966=CARTESIAN_POINT('Ctrl Pts',(-71.3125,6.58309518948457,-107.95));
#23967=CARTESIAN_POINT('Ctrl Pts',(-71.4995507654576,6.06724049855579,-107.927825180321));
#23968=CARTESIAN_POINT('Ctrl Pts',(-71.8031162620164,5.21219142607177,-107.854823997106));
#23969=CARTESIAN_POINT('Ctrl Pts',(-72.1125000002033,4.23816712577613,-107.560861613326));
#23970=CARTESIAN_POINT('Ctrl Pts',(-72.1125,3.42868316199158,-107.149999999604));
#23971=CARTESIAN_POINT('Ctrl Pts',(-71.3746924970224,6.02164757478294,-107.935082460943));
#23972=CARTESIAN_POINT('Ctrl Pts',(-71.6811438088394,5.16661471749831,-107.883111714002));
#23973=CARTESIAN_POINT('Ctrl Pts',(-72.0098408305469,4.19555805202373,-107.611458539987));
#23974=CARTESIAN_POINT('Ctrl Pts',(-72.0395269177012,3.39266652940126,-107.206172926527));
#23975=CARTESIAN_POINT('Ctrl Pts',(-71.2498342285872,5.97605465101008,-107.942339741564));
#23976=CARTESIAN_POINT('Ctrl Pts',(-71.5591713556625,5.12103800892486,-107.911399430897));
#23977=CARTESIAN_POINT('Ctrl Pts',(-71.9071816608906,4.15294897827133,-107.662055466649));
#23978=CARTESIAN_POINT('Ctrl Pts',(-71.9665538354024,3.35664989681094,-107.262345853449));
#23979=CARTESIAN_POINT('Ctrl Pts',(-71.124975960152,5.93046172723723,-107.949597022186));
#23980=CARTESIAN_POINT('Ctrl Pts',(-71.4371989024855,5.0754613003514,-107.939687147793));
#23981=CARTESIAN_POINT('Ctrl Pts',(-71.8045224912342,4.11033990451893,-107.71265239331));
#23982=CARTESIAN_POINT('Ctrl Pts',(-71.8935807531036,3.32063326422062,-107.318518780371));
#23983=CARTESIAN_POINT('',(-72.1125,3.42868316190273,-107.14999999978));
#23984=CARTESIAN_POINT('',(-71.8935807531036,3.32063326422075,-107.318518780371));
#23985=CARTESIAN_POINT('Ctrl Pts',(-72.1125,3.42868316199158,-107.149999999604));
#23986=CARTESIAN_POINT('Ctrl Pts',(-72.1125000002033,4.23816712577613,-107.560861613326));
#23987=CARTESIAN_POINT('Ctrl Pts',(-71.8031162620164,5.21219142607177,-107.854823997106));
#23988=CARTESIAN_POINT('Ctrl Pts',(-71.4995507654576,6.06724049855579,-107.927825180321));
#23989=CARTESIAN_POINT('Origin',(-72.0125,6.00000000000001,-101.95));
#23990=CARTESIAN_POINT('',(-72.1125,0.97333333333333,-104.843548379105));
#23991=CARTESIAN_POINT('',(-71.9125,0.800000000000001,-104.943325909419));
#23992=CARTESIAN_POINT('',(-72.1125,3.10645162089483,-106.976666666667));
#23993=CARTESIAN_POINT('Origin',(-72.1125,6.00000000000001,-101.95));
#23994=CARTESIAN_POINT('',(-72.1125,3.10645162089483,-106.976666666667));
#23995=CARTESIAN_POINT('Ctrl Pts',(-72.1125,3.4286831619917,-107.149999999604));
#23996=CARTESIAN_POINT('Ctrl Pts',(-72.1125,3.31801931336453,-107.093831465749));
#23997=CARTESIAN_POINT('Ctrl Pts',(-72.1125,3.21069598181733,-107.036673848678));
#23998=CARTESIAN_POINT('Ctrl Pts',(-72.1125,3.10645162089484,-106.976666666667));
#23999=CARTESIAN_POINT('Ctrl Pts',(-72.0395269177012,3.39266652940138,-107.206172926527));
#24000=CARTESIAN_POINT('Ctrl Pts',(-72.0435852768747,3.28290392767118,-107.150766682816));
#24001=CARTESIAN_POINT('Ctrl Pts',(-72.0458333333333,3.1763983554736,-107.093853853762));
#24002=CARTESIAN_POINT('Ctrl Pts',(-72.0458333333333,3.07319244412351,-107.034444444444));
#24003=CARTESIAN_POINT('Ctrl Pts',(-71.9665538354024,3.35664989681107,-107.262345853449));
#24004=CARTESIAN_POINT('Ctrl Pts',(-71.9746705537493,3.24778854197784,-107.207701899883));
#24005=CARTESIAN_POINT('Ctrl Pts',(-71.9791666666667,3.14210072912987,-107.151033858845));
#24006=CARTESIAN_POINT('Ctrl Pts',(-71.9791666666667,3.03993326735219,-107.092222222222));
#24007=CARTESIAN_POINT('Ctrl Pts',(-71.8935807531036,3.32063326422075,-107.318518780371));
#24008=CARTESIAN_POINT('Ctrl Pts',(-71.905755830624,3.2126731562845,-107.26463711695));
#24009=CARTESIAN_POINT('Ctrl Pts',(-71.9125,3.10780310278613,-107.208213863928));
#24010=CARTESIAN_POINT('Ctrl Pts',(-71.9125,3.00667409058086,-107.15));
#24011=CARTESIAN_POINT('Ctrl Pts',(-72.1125,3.10645162089484,-106.976666666667));
#24012=CARTESIAN_POINT('Ctrl Pts',(-72.1125,3.21069598181733,-107.036673848678));
#24013=CARTESIAN_POINT('Ctrl Pts',(-72.1125,3.31801931336453,-107.093831465749));
#24014=CARTESIAN_POINT('Ctrl Pts',(-72.1125,3.4286831619917,-107.149999999604));
#24015=CARTESIAN_POINT('Ctrl Pts',(-72.1125,0.800000000395794,-104.521316838008));
#24016=CARTESIAN_POINT('Ctrl Pts',(-72.1125000002033,0.389138161249151,
-103.71183243009));
#24017=CARTESIAN_POINT('Ctrl Pts',(-71.8031182842413,0.0951762823709496,
-102.737814086272));
#24018=CARTESIAN_POINT('Ctrl Pts',(-71.4995502644836,0.022174699205149,
-101.882758090414));
#24019=CARTESIAN_POINT('Ctrl Pts',(-72.0395269177012,0.74382707347345,-104.557333470599));
#24020=CARTESIAN_POINT('Ctrl Pts',(-72.0098408142592,0.338541237647051,
-103.754441507459));
#24021=CARTESIAN_POINT('Ctrl Pts',(-71.6811442271336,0.0668883759257339,
-102.783386394673));
#24022=CARTESIAN_POINT('Ctrl Pts',(-71.374691992172,0.0149174533184618,
-101.92835101664));
#24023=CARTESIAN_POINT('Ctrl Pts',(-71.9665538354024,0.687654146551105,
-104.593350103189));
#24024=CARTESIAN_POINT('Ctrl Pts',(-71.9071816283152,0.287944314044952,
-103.797050584828));
#24025=CARTESIAN_POINT('Ctrl Pts',(-71.5591701700259,0.0386004694805184,
-102.828958703074));
#24026=CARTESIAN_POINT('Ctrl Pts',(-71.2498337198604,0.00766020743177456,
-101.973943942866));
#24027=CARTESIAN_POINT('Ctrl Pts',(-71.8935807531036,0.63148121962876,-104.629366735779));
#24028=CARTESIAN_POINT('Ctrl Pts',(-71.8045224423712,0.237347390442852,
-103.839659662198));
#24029=CARTESIAN_POINT('Ctrl Pts',(-71.4371961129181,0.0103125630353027,
-102.874531011475));
#24030=CARTESIAN_POINT('Ctrl Pts',(-71.1249754475488,0.000402961545087344,
-102.019536869091));
#24031=CARTESIAN_POINT('',(-72.1125,0.800000000220446,-104.521316838097));
#24032=CARTESIAN_POINT('Ctrl Pts',(-71.4995502644836,0.022174699205149,
-101.882758090414));
#24033=CARTESIAN_POINT('Ctrl Pts',(-71.8031182842413,0.0951762823709496,
-102.737814086272));
#24034=CARTESIAN_POINT('Ctrl Pts',(-72.1125000002033,0.389138161249151,
-103.71183243009));
#24035=CARTESIAN_POINT('Ctrl Pts',(-72.1125,0.800000000395794,-104.521316838008));
#24036=CARTESIAN_POINT('',(-72.1125,0.800000000220446,-104.521316838097));
#24037=CARTESIAN_POINT('Ctrl Pts',(-72.1125,0.973333333333336,-104.843548379105));
#24038=CARTESIAN_POINT('Ctrl Pts',(-72.1125,0.913326151321781,-104.739304018183));
#24039=CARTESIAN_POINT('Ctrl Pts',(-72.1125,0.856168534250963,-104.631980686636));
#24040=CARTESIAN_POINT('Ctrl Pts',(-72.1125,0.800000000395737,-104.521316838008));
#24041=CARTESIAN_POINT('Ctrl Pts',(-72.0458333333333,0.915555555555558,
-104.876807555876));
#24042=CARTESIAN_POINT('Ctrl Pts',(-72.0458333333333,0.856146146238371,
-104.773601644526));
#24043=CARTESIAN_POINT('Ctrl Pts',(-72.0435852768747,0.799233317184014,
-104.667096072329));
#24044=CARTESIAN_POINT('Ctrl Pts',(-72.0395269177012,0.743827073473394,
-104.557333470599));
#24045=CARTESIAN_POINT('Ctrl Pts',(-71.9791666666667,0.85777777777778,-104.910066732648));
#24046=CARTESIAN_POINT('Ctrl Pts',(-71.9791666666667,0.798966141154961,
-104.80789927087));
#24047=CARTESIAN_POINT('Ctrl Pts',(-71.9746705537493,0.742298100117066,
-104.702211458022));
#24048=CARTESIAN_POINT('Ctrl Pts',(-71.9665538354024,0.68765414655105,-104.593350103189));
#24049=CARTESIAN_POINT('Ctrl Pts',(-71.9125,0.800000000000002,-104.943325909419));
#24050=CARTESIAN_POINT('Ctrl Pts',(-71.9125,0.741786136071551,-104.842196897214));
#24051=CARTESIAN_POINT('Ctrl Pts',(-71.905755830624,0.685362883050117,-104.737326843716));
#24052=CARTESIAN_POINT('Ctrl Pts',(-71.8935807531036,0.631481219628707,
-104.629366735779));
#24053=CARTESIAN_POINT('Ctrl Pts',(-72.1125,0.800000000395737,-104.521316838008));
#24054=CARTESIAN_POINT('Ctrl Pts',(-72.1125,0.856168534250963,-104.631980686636));
#24055=CARTESIAN_POINT('Ctrl Pts',(-72.1125,0.913326151321781,-104.739304018183));
#24056=CARTESIAN_POINT('Ctrl Pts',(-72.1125,0.973333333333336,-104.843548379105));
#24057=CARTESIAN_POINT('Origin',(-71.3125,0.800000000000001,-66.85));
#24058=CARTESIAN_POINT('',(-71.3125,5.55111512312578E-16,37.8669048105155));
#24059=CARTESIAN_POINT('',(-71.3125,0.,-66.85));
#24060=CARTESIAN_POINT('',(-71.4995507644729,0.0221748194419996,38.3827594987134));
#24061=CARTESIAN_POINT('Ctrl Pts',(-71.4995507644729,0.0221748194419995,
38.3827594987134));
#24062=CARTESIAN_POINT('Ctrl Pts',(-71.4990207956831,0.0220473729800413,
38.3812667424329));
#24063=CARTESIAN_POINT('Ctrl Pts',(-71.4984892431503,0.0219200770893842,
38.3797698452961));
#24064=CARTESIAN_POINT('Ctrl Pts',(-71.4979015355679,0.021780062829885,
38.378114793822));
#24065=CARTESIAN_POINT('Ctrl Pts',(-71.4972864937771,0.0216335365241201,
38.3763827661041));
#24066=CARTESIAN_POINT('Ctrl Pts',(-71.4966099607556,0.021473078866498,
38.3744775536761));
#24067=CARTESIAN_POINT('Ctrl Pts',(-71.4958284690637,0.0212890957288703,
38.3722769943803));
#24068=CARTESIAN_POINT('Ctrl Pts',(-71.4950181141868,0.02109831745909,38.3699951608361));
#24069=CARTESIAN_POINT('Ctrl Pts',(-71.4940949716375,0.0208822545381878,
38.3673959498629));
#24070=CARTESIAN_POINT('Ctrl Pts',(-71.4930300007572,0.0206355673841659,
38.3643985413472));
#24071=CARTESIAN_POINT('Ctrl Pts',(-71.4919169497944,0.0203777430817619,
38.3612658092734));
#24072=CARTESIAN_POINT('Ctrl Pts',(-71.4906490552782,0.0200864903833777,
38.3576983462725));
#24073=CARTESIAN_POINT('Ctrl Pts',(-71.4892128876169,0.0197612190168368,
38.3536601221728));
#24074=CARTESIAN_POINT('Ctrl Pts',(-71.4876933992894,0.0194170767150211,
38.349387616567));
#24075=CARTESIAN_POINT('Ctrl Pts',(-71.485985646331,0.0190349037745015,
38.3445884467408));
#24076=CARTESIAN_POINT('Ctrl Pts',(-71.4840939717242,0.0186194852263588,
38.3392774856718));
#24077=CARTESIAN_POINT('Ctrl Pts',(-71.4820490634828,0.0181704160208765,
38.33353631432));
#24078=CARTESIAN_POINT('Ctrl Pts',(-71.4797893694556,0.0176825937973,38.3271975203437));
#24079=CARTESIAN_POINT('Ctrl Pts',(-71.4773416119619,0.0171671679305936,
38.3203397199083));
#24080=CARTESIAN_POINT('Ctrl Pts',(-71.4745651240188,0.016582521082149,
38.3125609263497));
#24081=CARTESIAN_POINT('Ctrl Pts',(-71.4715469164779,0.0159625615450801,
38.3041151608526));
#24082=CARTESIAN_POINT('Ctrl Pts',(-71.4683495355182,0.0153275063577457,
38.295182272364));
#24083=CARTESIAN_POINT('Ctrl Pts',(-71.4633966211176,0.0143437718506017,
38.2813447495314));
#24084=CARTESIAN_POINT('Ctrl Pts',(-71.4580152337396,0.0133254515238729,
38.2663432691807));
#24085=CARTESIAN_POINT('Ctrl Pts',(-71.4524868440586,0.0123429150381997,
38.2509734082674));
#24086=CARTESIAN_POINT('Ctrl Pts',(-71.4489551985486,0.0117152511490301,
38.241154834792));
#24087=CARTESIAN_POINT('Ctrl Pts',(-71.4453646860824,0.0111019335359449,
38.2311887561521));
#24088=CARTESIAN_POINT('Ctrl Pts',(-71.4417814229731,0.010515159313331,
38.2212593972102));
#24089=CARTESIAN_POINT('Ctrl Pts',(-71.4384221138081,0.00996505847963049,
38.2119506232022));
#24090=CARTESIAN_POINT('Ctrl Pts',(-71.4350696915454,0.00943826368962347,
38.2026754960875));
#24091=CARTESIAN_POINT('Ctrl Pts',(-71.4317621917286,0.00893961695450685,
38.1935386637876));
#24092=CARTESIAN_POINT('Ctrl Pts',(-71.4288719604788,0.00850387864572192,
38.1855545187534));
#24093=CARTESIAN_POINT('Ctrl Pts',(-71.4260160518402,0.00808954564913643,
38.1776759881089));
#24094=CARTESIAN_POINT('Ctrl Pts',(-71.4232040488063,0.00769664043506357,
38.1699285344855));
#24095=CARTESIAN_POINT('Ctrl Pts',(-71.4205610599081,0.00732735060630408,
38.1626467379619));
#24096=CARTESIAN_POINT('Ctrl Pts',(-71.41795694981,0.00697694595537342,
38.1554809708886));
#24097=CARTESIAN_POINT('Ctrl Pts',(-71.4153837884622,0.00664325422186796,
38.1484081974271));
#24098=CARTESIAN_POINT('Ctrl Pts',(-71.4129144136961,0.00632302170046841,
38.1416206991121));
#24099=CARTESIAN_POINT('Ctrl Pts',(-71.4104736323363,0.00601814532745467,
38.1349190823032));
#24100=CARTESIAN_POINT('Ctrl Pts',(-71.4080379901782,0.00572517827095886,
38.1282375072849));
#24101=CARTESIAN_POINT('Ctrl Pts',(-71.4055526461237,0.0054262329067401,
38.1214195875458));
#24102=CARTESIAN_POINT('Ctrl Pts',(-71.4030698651113,0.00513933086078111,
38.1146148153011));
#24103=CARTESIAN_POINT('Ctrl Pts',(-71.4005585977608,0.00486121754727409,
38.1077364762525));
#24104=CARTESIAN_POINT('Ctrl Pts',(-71.3979671396617,0.0045742234131711,
38.1006384954532));
#24105=CARTESIAN_POINT('Ctrl Pts',(-71.3953454091284,0.00429665292678922,
38.0934623658199));
#24106=CARTESIAN_POINT('Ctrl Pts',(-71.392679653921,0.00402812669221708,
38.0861692117592));
#24107=CARTESIAN_POINT('Ctrl Pts',(-71.3898657603368,0.00374467821706666,
38.0784707706709));
#24108=CARTESIAN_POINT('Ctrl Pts',(-71.3870029206609,0.00347138520559411,
38.0706422519179));
#24109=CARTESIAN_POINT('Ctrl Pts',(-71.384095836396,0.00321016810531405,
38.0626954692138));
#24110=CARTESIAN_POINT('Ctrl Pts',(-71.3809669976009,0.00292902517211406,
38.0541425000684));
#24111=CARTESIAN_POINT('Ctrl Pts',(-71.3777870650587,0.00266197605738847,
38.0454529881455));
#24112=CARTESIAN_POINT('Ctrl Pts',(-71.3745834568822,0.00241261019148575,
38.036700791836));
#24113=CARTESIAN_POINT('Ctrl Pts',(-71.3709749451015,0.00213172700751753,
38.0268424066186));
#24114=CARTESIAN_POINT('Ctrl Pts',(-71.3673366707961,0.00187344761883645,
38.0169052583702));
#24115=CARTESIAN_POINT('Ctrl Pts',(-71.3637310438776,0.0016420726621369,
38.0070583422105));
#24116=CARTESIAN_POINT('Ctrl Pts',(-71.356940177458,0.00120629922819576,
37.9885125819873));
#24117=CARTESIAN_POINT('Ctrl Pts',(-71.3502675171857,0.000869036069561573,
37.9702933137546));
#24118=CARTESIAN_POINT('Ctrl Pts',(-71.3442156403977,0.000628923369027201,
37.9537634911982));
#24119=CARTESIAN_POINT('Ctrl Pts',(-71.3411205066207,0.000506121640610308,
37.9453095827801));
#24120=CARTESIAN_POINT('Ctrl Pts',(-71.3381883477706,0.000407933340316306,
37.9372992320297));
#24121=CARTESIAN_POINT('Ctrl Pts',(-71.3354757471578,0.000329996159329049,
37.9298861299241));
#24122=CARTESIAN_POINT('Ctrl Pts',(-71.3330312432178,0.000259761807429823,
37.9232056929958));
#24123=CARTESIAN_POINT('Ctrl Pts',(-71.330765274502,0.00020588491124297,
37.9170109178627));
#24124=CARTESIAN_POINT('Ctrl Pts',(-71.328704924838,0.000164141582166488,
37.9113755218124));
#24125=CARTESIAN_POINT('Ctrl Pts',(-71.3267779827721,0.0001251011327827,
37.9061050175396));
#24126=CARTESIAN_POINT('Ctrl Pts',(-71.3250310435743,9.66253253805291E-5,
37.9013242110388));
#24127=CARTESIAN_POINT('Ctrl Pts',(-71.3234704632832,7.52229519629388E-5,
37.8970505378663));
#24128=CARTESIAN_POINT('Ctrl Pts',(-71.3220188855637,5.53154799969384E-5,
37.8930753699158));
#24129=CARTESIAN_POINT('Ctrl Pts',(-71.3207285827801,4.15083061174377E-5,
37.889539080621));
#24130=CARTESIAN_POINT('Ctrl Pts',(-71.3195893260971,3.1412207024184E-5,
37.8864139746195));
#24131=CARTESIAN_POINT('Ctrl Pts',(-71.3184846159629,2.16222596392345E-5,
37.8833836335894));
#24132=CARTESIAN_POINT('Ctrl Pts',(-71.3175220329355,1.53159280140433E-5,
37.880740200413));
#24133=CARTESIAN_POINT('Ctrl Pts',(-71.3166761339687,1.09001335865111E-5,
37.8784145222705));
#24134=CARTESIAN_POINT('Ctrl Pts',(-71.3158524584221,6.60035071474075E-6,
37.8761499442413));
#24135=CARTESIAN_POINT('Ctrl Pts',(-71.3151395029899,4.09626587467967E-6,
37.8741868830752));
#24136=CARTESIAN_POINT('Ctrl Pts',(-71.3144968795844,2.49220892911683E-6,
37.8724154152659));
#24137=CARTESIAN_POINT('Ctrl Pts',(-71.3138743484812,9.38304525135002E-7,
37.8706993342765));
#24138=CARTESIAN_POINT('Ctrl Pts',(-71.3133178685519,2.32998667997062E-7,
37.8691631867836));
#24139=CARTESIAN_POINT('Ctrl Pts',(-71.31277370762,4.68224151672914E-8,
37.8676606128799));
#24140=CARTESIAN_POINT('Ctrl Pts',(-71.3126822667669,1.55373405006649E-8,
37.8674081202228));
#24141=CARTESIAN_POINT('Ctrl Pts',(-71.3125911327533,5.5612328912237E-16,
37.867156463649));
#24142=CARTESIAN_POINT('Ctrl Pts',(-71.3125,5.55111512312578E-16,37.8669048105155));
#24143=CARTESIAN_POINT('',(-72.1125,0.800000000220445,41.0213168380973));
#24144=CARTESIAN_POINT('Ctrl Pts',(-72.1125,0.800000000395795,41.0213168380085));
#24145=CARTESIAN_POINT('Ctrl Pts',(-72.1125000002033,0.389138386673939,
40.2118328742239));
#24146=CARTESIAN_POINT('Ctrl Pts',(-71.8031180421414,0.095176430570246,
39.2378135490065));
#24147=CARTESIAN_POINT('Ctrl Pts',(-71.4995507644729,0.0221748194419993,
38.3827594987134));
#24148=CARTESIAN_POINT('',(-72.1125,0.800000000000001,-66.85));
#24149=CARTESIAN_POINT('Origin',(-67.35,0.,-101.95));
#24150=CARTESIAN_POINT('',(-68.15,0.,-66.85));
#24151=CARTESIAN_POINT('',(-71.099583741031,2.22044604925031E-15,38.45));
#24152=CARTESIAN_POINT('',(-67.35,2.22044604925031E-15,38.45));
#24153=CARTESIAN_POINT('',(-71.2060418705155,1.38777878078145E-15,38.1584524052577));
#24154=CARTESIAN_POINT('Ctrl Pts',(-71.4995502651826,6.06724190764745,44.4278253006268));
#24155=CARTESIAN_POINT('Ctrl Pts',(-71.4893114124994,6.09608154849019,44.4302875246095));
#24156=CARTESIAN_POINT('Ctrl Pts',(-71.3975276772687,6.35256309319244,44.4503655595348));
#24157=CARTESIAN_POINT('Ctrl Pts',(-71.3203476800974,6.56142467898143,44.45));
#24158=CARTESIAN_POINT('Ctrl Pts',(-71.3125,6.58309518948451,44.45));
#24159=CARTESIAN_POINT('Ctrl Pts',(-71.3746919924042,6.02164898271828,44.435082546577));
#24160=CARTESIAN_POINT('Ctrl Pts',(-71.3673450818445,6.04220422326533,44.4361237366707));
#24161=CARTESIAN_POINT('Ctrl Pts',(-71.3026150186436,6.22408187278844,44.4524101433031));
#24162=CARTESIAN_POINT('Ctrl Pts',(-71.2471140006817,6.37331286135218,44.45));
#24163=CARTESIAN_POINT('Ctrl Pts',(-71.241527913677,6.38873012632301,44.45));
#24164=CARTESIAN_POINT('Ctrl Pts',(-71.2498337196257,5.97605605778911,44.4423397925273));
#24165=CARTESIAN_POINT('Ctrl Pts',(-71.2454420638959,5.98825113903958,44.4425732724023));
#24166=CARTESIAN_POINT('Ctrl Pts',(-71.2057778485336,6.09746688787165,44.4476681728695));
#24167=CARTESIAN_POINT('Ctrl Pts',(-71.173880321266,6.18520104372293,44.45));
#24168=CARTESIAN_POINT('Ctrl Pts',(-71.170555827354,6.1943650631615,44.45));
#24169=CARTESIAN_POINT('Ctrl Pts',(-71.1249754468472,5.93046313285994,44.4495970384775));
#24170=CARTESIAN_POINT('Ctrl Pts',(-71.1235583328476,5.93434379913903,44.4496420163942));
#24171=CARTESIAN_POINT('Ctrl Pts',(-71.1109271247571,5.96893411817337,44.4500077127941));
#24172=CARTESIAN_POINT('Ctrl Pts',(-71.1006466418503,5.99708922609368,44.45));
#24173=CARTESIAN_POINT('Ctrl Pts',(-71.099583741031,6.,44.45));
#24174=CARTESIAN_POINT('',(-71.4995502651826,6.06724190764745,44.4278253006268));
#24175=CARTESIAN_POINT('Ctrl Pts',(-71.3125,6.58309518948451,44.45));
#24176=CARTESIAN_POINT('Ctrl Pts',(-71.3130414730319,6.58159997091307,44.45));
#24177=CARTESIAN_POINT('Ctrl Pts',(-71.3135844616982,6.58010061545634,44.4499994907131));
#24178=CARTESIAN_POINT('Ctrl Pts',(-71.3141854581767,6.57844322897758,44.4499982245172));
#24179=CARTESIAN_POINT('Ctrl Pts',(-71.3148143991277,6.57670877916745,44.4499968994472));
#24180=CARTESIAN_POINT('Ctrl Pts',(-71.3155068597438,6.57480128397541,44.449994750064));
#24181=CARTESIAN_POINT('Ctrl Pts',(-71.3163076849504,6.57259867099708,44.4499909384083));
#24182=CARTESIAN_POINT('Ctrl Pts',(-71.31713807453,6.57031474330561,44.4499869860361));
#24183=CARTESIAN_POINT('Ctrl Pts',(-71.3180849093956,6.56771369413082,44.4499812519661));
#24184=CARTESIAN_POINT('Ctrl Pts',(-71.3191778993281,6.56471475376676,44.4499721280523));
#24185=CARTESIAN_POINT('Ctrl Pts',(-71.3203202083267,6.5615804919933,44.4499625924395));
#24186=CARTESIAN_POINT('Ctrl Pts',(-71.3216220762682,6.55801185344091,44.4499493502156));
#24187=CARTESIAN_POINT('Ctrl Pts',(-71.3230967980082,6.55397281294346,44.4499298143412));
#24188=CARTESIAN_POINT('Ctrl Pts',(-71.3246570200264,6.54969960007501,44.449909145831));
#24189=CARTESIAN_POINT('Ctrl Pts',(-71.3264106108636,6.54490016320096,44.4498814075098));
#24190=CARTESIAN_POINT('Ctrl Pts',(-71.3283521807648,6.53958932246207,44.4498429273082));
#24191=CARTESIAN_POINT('Ctrl Pts',(-71.3304508793576,6.53384868238601,44.4498013329547));
#24192=CARTESIAN_POINT('Ctrl Pts',(-71.3327690552956,6.52751095521831,44.4497471254782));
#24193=CARTESIAN_POINT('Ctrl Pts',(-71.3352778810258,6.52065461386513,44.449675664339));
#24194=CARTESIAN_POINT('Ctrl Pts',(-71.3381228093806,6.51287974146511,44.4495946296865));
#24195=CARTESIAN_POINT('Ctrl Pts',(-71.3412126011462,6.50443878957283,44.4494912678601));
#24196=CARTESIAN_POINT('Ctrl Pts',(-71.3444812014443,6.49551117516062,44.4493604961181));
#24197=CARTESIAN_POINT('Ctrl Pts',(-71.3495556188186,6.48165128482434,44.4491574763729));
#24198=CARTESIAN_POINT('Ctrl Pts',(-71.3550592025856,6.46662336130317,44.4488871120809));
#24199=CARTESIAN_POINT('Ctrl Pts',(-71.3606972674011,6.45122664552515,44.4485468198015));
#24200=CARTESIAN_POINT('Ctrl Pts',(-71.3642934132123,6.44140610660548,44.4483297700344));
#24201=CARTESIAN_POINT('Ctrl Pts',(-71.3679432201769,6.43143836252666,44.4480847940351));
#24202=CARTESIAN_POINT('Ctrl Pts',(-71.3715786926663,6.42150762201508,44.4478155852532));
#24203=CARTESIAN_POINT('Ctrl Pts',(-71.3749869481252,6.41219755278548,44.4475632020201));
#24204=CARTESIAN_POINT('Ctrl Pts',(-71.3783821050343,6.40292137962196,44.4472896652331));
#24205=CARTESIAN_POINT('Ctrl Pts',(-71.3817254153414,6.39378372955202,44.4469992734443));
#24206=CARTESIAN_POINT('Ctrl Pts',(-71.3846464426477,6.38580022729881,44.4467455601284));
#24207=CARTESIAN_POINT('Ctrl Pts',(-71.387527894579,6.37792247617558,44.4464790726766));
#24208=CARTESIAN_POINT('Ctrl Pts',(-71.3903601144382,6.37017591351312,44.4462021116398));
#24209=CARTESIAN_POINT('Ctrl Pts',(-71.3930216639747,6.36289616077923,44.4459418403488));
#24210=CARTESIAN_POINT('Ctrl Pts',(-71.3956396564043,6.35573249576139,44.4456723848728));
#24211=CARTESIAN_POINT('Ctrl Pts',(-71.3982221077352,6.34866190828219,44.445394066011));
#24212=CARTESIAN_POINT('Ctrl Pts',(-71.4007009278315,6.34187505653155,44.4451269158115));
#24213=CARTESIAN_POINT('Ctrl Pts',(-71.4031469208213,6.3351742015686,44.4448516557739));
#24214=CARTESIAN_POINT('Ctrl Pts',(-71.4055836100285,6.32849354473077,44.4445661970812));
#24215=CARTESIAN_POINT('Ctrl Pts',(-71.4080709304171,6.32167407267327,44.4442748069341));
#24216=CARTESIAN_POINT('Ctrl Pts',(-71.4105513495158,6.31486792632762,44.4439724845748));
#24217=CARTESIAN_POINT('Ctrl Pts',(-71.4130558872244,6.30798832458474,44.4436551603464));
#24218=CARTESIAN_POINT('Ctrl Pts',(-71.4156402710321,6.30088939719107,44.4433277196396));
#24219=CARTESIAN_POINT('Ctrl Pts',(-71.4182502612752,6.29371244739847,44.4429842570855));
#24220=CARTESIAN_POINT('Ctrl Pts',(-71.4208995017854,6.28641857841381,44.4426219452));
#24221=CARTESIAN_POINT('Ctrl Pts',(-71.4236959667089,6.2787193722855,44.4422394988064));
#24222=CARTESIAN_POINT('Ctrl Pts',(-71.4265360438204,6.27089020577405,44.4418359995615));
#24223=CARTESIAN_POINT('Ctrl Pts',(-71.4294150367517,6.2629429051824,44.4414106861683));
#24224=CARTESIAN_POINT('Ctrl Pts',(-71.432513653979,6.2543893438808,44.4409529276955));
#24225=CARTESIAN_POINT('Ctrl Pts',(-71.4356571739941,6.24569938969948,44.4404698354042));
#24226=CARTESIAN_POINT('Ctrl Pts',(-71.4388186030689,6.23694695263107,44.4399643096487));
#24227=CARTESIAN_POINT('Ctrl Pts',(-71.4423797435989,6.22708791178466,44.4393948683567));
#24228=CARTESIAN_POINT('Ctrl Pts',(-71.4459633037202,6.21715035833354,44.4387968648388));
#24229=CARTESIAN_POINT('Ctrl Pts',(-71.449508394624,6.20730341158804,44.4381806263811));
#24230=CARTESIAN_POINT('Ctrl Pts',(-71.4561832905068,6.18876302825965,44.4370203380683));
#24231=CARTESIAN_POINT('Ctrl Pts',(-71.462718828944,6.17055030095169,44.4357930115265));
#24232=CARTESIAN_POINT('Ctrl Pts',(-71.4686322750488,6.15402777629251,44.4346162837261));
#24233=CARTESIAN_POINT('Ctrl Pts',(-71.4716575881422,6.14557486925647,44.4340142709641));
#24234=CARTESIAN_POINT('Ctrl Pts',(-71.4745196697734,6.13756600214882,44.4334264063996));
#24235=CARTESIAN_POINT('Ctrl Pts',(-71.4771650503419,6.13015493599191,44.4328699899702));
#24236=CARTESIAN_POINT('Ctrl Pts',(-71.4795488948579,6.12347656629865,44.4323685837568));
#24237=CARTESIAN_POINT('Ctrl Pts',(-71.4817565642925,6.1172842734726,44.4318928535763));
#24238=CARTESIAN_POINT('Ctrl Pts',(-71.4837629722623,6.11165176399895,44.4314531299649));
#24239=CARTESIAN_POINT('Ctrl Pts',(-71.48563944169,6.10638402583829,44.4310418836352));
#24240=CARTESIAN_POINT('Ctrl Pts',(-71.4873397401627,6.10160632696767,44.4306622124859));
#24241=CARTESIAN_POINT('Ctrl Pts',(-71.4888585907838,6.09733604160017,44.4303189395733));
#24242=CARTESIAN_POINT('Ctrl Pts',(-71.4902713563202,6.09336401702186,44.4299996427749));
#24243=CARTESIAN_POINT('Ctrl Pts',(-71.4915271008574,6.08983111529501,44.4297118654696));
#24244=CARTESIAN_POINT('Ctrl Pts',(-71.4926362835771,6.08670954431889,44.4294555274928));
#24245=CARTESIAN_POINT('Ctrl Pts',(-71.4937118264108,6.08368264601486,44.4292069638711));
#24246=CARTESIAN_POINT('Ctrl Pts',(-71.4946494646873,6.08104279063262,44.4289879910269));
#24247=CARTESIAN_POINT('Ctrl Pts',(-71.4954741515926,6.07872068925268,44.4287942346018));
#24248=CARTESIAN_POINT('Ctrl Pts',(-71.4962771694046,6.0764596023391,44.4286055692312));
#24249=CARTESIAN_POINT('Ctrl Pts',(-71.4969730091871,6.07450002927982,44.4284408297404));
#24250=CARTESIAN_POINT('Ctrl Pts',(-71.4976008840125,6.07273187234974,44.4282915024191));
#24251=CARTESIAN_POINT('Ctrl Pts',(-71.4982091353165,6.07101897717568,44.4281468421553));
#24252=CARTESIAN_POINT('Ctrl Pts',(-71.498753555852,6.06948585391535,44.4280166533539));
#24253=CARTESIAN_POINT('Ctrl Pts',(-71.4992861074866,6.06798592939874,44.427888777429));
#24254=CARTESIAN_POINT('Ctrl Pts',(-71.4993743533654,6.06773738606794,44.4278675878905));
#24255=CARTESIAN_POINT('Ctrl Pts',(-71.499462311639,6.06748964522966,44.4278464515634));
#24256=CARTESIAN_POINT('Ctrl Pts',(-71.4995502651826,6.06724190764745,44.4278253006268));
#24257=CARTESIAN_POINT('',(-71.1249754468472,5.93046313285994,44.4495970384775));
#24258=CARTESIAN_POINT('Ctrl Pts',(-71.1249754468472,5.93046313285994,44.4495970384775));
#24259=CARTESIAN_POINT('Ctrl Pts',(-71.2498337196257,5.97605605778911,44.4423397925273));
#24260=CARTESIAN_POINT('Ctrl Pts',(-71.3746919924042,6.02164898271828,44.435082546577));
#24261=CARTESIAN_POINT('Ctrl Pts',(-71.4995502651826,6.06724190764745,44.4278253006268));
#24262=CARTESIAN_POINT('Ctrl Pts',(-71.1249754468472,5.93046313285994,44.4495970384775));
#24263=CARTESIAN_POINT('Ctrl Pts',(-71.1248515871029,5.93080231399357,44.4496009696738));
#24264=CARTESIAN_POINT('Ctrl Pts',(-71.1247261187253,5.93114590045165,44.4496049290215));
#24265=CARTESIAN_POINT('Ctrl Pts',(-71.1245663839378,5.93158332280883,44.4496099171765));
#24266=CARTESIAN_POINT('Ctrl Pts',(-71.124399215446,5.93204110183689,44.4496151374692));
#24267=CARTESIAN_POINT('Ctrl Pts',(-71.1241946568714,5.93260127070091,44.4496214810533));
#24268=CARTESIAN_POINT('Ctrl Pts',(-71.1239352648988,5.93331159796484,44.4496293766394));
#24269=CARTESIAN_POINT('Ctrl Pts',(-71.1236418501879,5.9341150941825,44.4496383078375));
#24270=CARTESIAN_POINT('Ctrl Pts',(-71.1232782835419,5.93511069785848,44.4496492227469));
#24271=CARTESIAN_POINT('Ctrl Pts',(-71.1228435341425,5.93630123568408,44.4496618627573));
#24272=CARTESIAN_POINT('Ctrl Pts',(-71.1223678608009,5.93760384152227,44.4496756926004));
#24273=CARTESIAN_POINT('Ctrl Pts',(-71.1218074187549,5.93913858691462,44.4496915586601));
#24274=CARTESIAN_POINT('Ctrl Pts',(-71.1211844497222,5.94084456975602,44.4497083791692));
#24275=CARTESIAN_POINT('Ctrl Pts',(-71.1202527747972,5.94339593483545,44.4497335349083));
#24276=CARTESIAN_POINT('Ctrl Pts',(-71.1191829294765,5.94632569724299,44.4497606651809));
#24277=CARTESIAN_POINT('Ctrl Pts',(-71.1180892995269,5.94932062429705,44.4497859629222));
#24278=CARTESIAN_POINT('Ctrl Pts',(-71.1173517755765,5.95134034809186,44.4498030232543));
#24279=CARTESIAN_POINT('Ctrl Pts',(-71.1166045454595,5.95338666559846,44.4498192636616));
#24280=CARTESIAN_POINT('Ctrl Pts',(-71.1158742947463,5.95538649749497,44.4498341339902));
#24281=CARTESIAN_POINT('Ctrl Pts',(-71.1152379642737,5.95712912362704,44.449847091791));
#24282=CARTESIAN_POINT('Ctrl Pts',(-71.1146147683738,5.95883579007516,44.4498590203309));
#24283=CARTESIAN_POINT('Ctrl Pts',(-71.114008582509,5.9604958820991,44.4498699506463));
#24284=CARTESIAN_POINT('Ctrl Pts',(-71.1134416131077,5.96204857647174,44.4498801738382));
#24285=CARTESIAN_POINT('Ctrl Pts',(-71.1128897129432,5.96356001028047,44.4498895316588));
#24286=CARTESIAN_POINT('Ctrl Pts',(-71.1123401813906,5.96506496295198,44.4498982944035));
#24287=CARTESIAN_POINT('Ctrl Pts',(-71.1117897476999,5.96657238622816,44.4499070715337));
#24288=CARTESIAN_POINT('Ctrl Pts',(-71.1112385931528,5.96808178899618,44.4499153019222));
#24289=CARTESIAN_POINT('Ctrl Pts',(-71.1106726306169,5.96963174796688,44.4499231469468));
#24290=CARTESIAN_POINT('Ctrl Pts',(-71.1100599015201,5.97130978299583,44.4499316402207));
#24291=CARTESIAN_POINT('Ctrl Pts',(-71.1094299980603,5.97303485537856,44.4499396657415));
#24292=CARTESIAN_POINT('Ctrl Pts',(-71.1087859002502,5.97479880212128,44.4499470747354));
#24293=CARTESIAN_POINT('Ctrl Pts',(-71.1080330495214,5.97686058306483,44.4499557347034));
#24294=CARTESIAN_POINT('Ctrl Pts',(-71.1072611033227,5.97897466126154,44.4499635242262));
#24295=CARTESIAN_POINT('Ctrl Pts',(-71.10649893061,5.98106197314173,44.4499701125205));
#24296=CARTESIAN_POINT('Ctrl Pts',(-71.1055840057745,5.98356761713372,44.4499780212187));
#24297=CARTESIAN_POINT('Ctrl Pts',(-71.1046847838885,5.98603025599151,44.4499841533453));
#24298=CARTESIAN_POINT('Ctrl Pts',(-71.1038687720391,5.98826500948254,44.4499885241555));
#24299=CARTESIAN_POINT('Ctrl Pts',(-71.1032398030133,5.98998752212432,44.4499918931068));
#24300=CARTESIAN_POINT('Ctrl Pts',(-71.1026610568414,5.99157249064109,44.4499942405047));
#24301=CARTESIAN_POINT('Ctrl Pts',(-71.1021565447218,5.99295415655121,44.4499958630061));
#24302=CARTESIAN_POINT('Ctrl Pts',(-71.101698261038,5.99420922044048,44.4499973368377));
#24303=CARTESIAN_POINT('Ctrl Pts',(-71.1013015496871,5.99529565802496,44.4499982237945));
#24304=CARTESIAN_POINT('Ctrl Pts',(-71.1009716247545,5.99619919007953,44.4499987961535));
#24305=CARTESIAN_POINT('Ctrl Pts',(-71.1006620428143,5.99704701083741,44.4499993332212));
#24306=CARTESIAN_POINT('Ctrl Pts',(-71.1004114664506,5.9977332351973,44.4499995974697));
#24307=CARTESIAN_POINT('Ctrl Pts',(-71.1002088601892,5.99828808589258,44.4499997557792));
#24308=CARTESIAN_POINT('Ctrl Pts',(-71.1000192696623,5.99880729213499,44.4499999039186));
#24309=CARTESIAN_POINT('Ctrl Pts',(-71.0998717695326,5.99921122722298,44.4499999587511));
#24310=CARTESIAN_POINT('Ctrl Pts',(-71.0997415471272,5.99956784464617,44.4499999844368));
#24311=CARTESIAN_POINT('Ctrl Pts',(-71.0996870475666,5.99971709310149,44.4499999951866));
#24312=CARTESIAN_POINT('Ctrl Pts',(-71.0996353689454,5.99985861598442,44.45));
#24313=CARTESIAN_POINT('Ctrl Pts',(-71.099583741031,6.,44.45));
#24314=CARTESIAN_POINT('Ctrl Pts',(-71.1249759611403,0.0004029778460235,
38.5195382755115));
#24315=CARTESIAN_POINT('Ctrl Pts',(-71.124444532618,0.000386110444049271,
38.5180829961864));
#24316=CARTESIAN_POINT('Ctrl Pts',(-71.1227760188122,0.000327740135672606,
38.5135139660428));
#24317=CARTESIAN_POINT('Ctrl Pts',(-71.1158413990602,0.00015687896315957,
38.4945235499686));
#24318=CARTESIAN_POINT('Ctrl Pts',(-71.1102309858307,5.99412278512498E-5,
38.4791587927645));
#24319=CARTESIAN_POINT('Ctrl Pts',(-71.1041805090849,7.89965273412722E-6,
38.462588711091));
#24320=CARTESIAN_POINT('Ctrl Pts',(-71.1006150014995,-2.20980597269683E-7,
38.4528241478644));
#24321=CARTESIAN_POINT('Ctrl Pts',(-71.0999380484808,2.22118770383862E-15,
38.4509702776222));
#24322=CARTESIAN_POINT('Ctrl Pts',(-71.099583741031,2.22044604925032E-15,
38.45));
#24323=CARTESIAN_POINT('Ctrl Pts',(-71.2498342289178,0.00766025837801554,
38.4739453499121));
#24324=CARTESIAN_POINT('Ctrl Pts',(-71.2481873474268,0.00757270113481584,
38.4693721648531));
#24325=CARTESIAN_POINT('Ctrl Pts',(-71.2417364154876,0.00689152341476491,
38.4515647287784));
#24326=CARTESIAN_POINT('Ctrl Pts',(-71.2226921830148,0.00496933901996202,
38.3991367663831));
#24327=CARTESIAN_POINT('Ctrl Pts',(-71.2027396366171,0.00276041256014256,
38.344204338792));
#24328=CARTESIAN_POINT('Ctrl Pts',(-71.1853003558039,0.00110280150098152,
38.2962243229244));
#24329=CARTESIAN_POINT('Ctrl Pts',(-71.1746388922473,0.000211812862022938,
38.2668856359242));
#24330=CARTESIAN_POINT('Ctrl Pts',(-71.1716639991687,1.6754385265044E-15,
38.2586896296946));
#24331=CARTESIAN_POINT('Ctrl Pts',(-71.170555827354,1.66533453693774E-15,
38.2556349368385));
#24332=CARTESIAN_POINT('Ctrl Pts',(-71.3746924966954,0.0149175389100076,
38.4283524243128));
#24333=CARTESIAN_POINT('Ctrl Pts',(-71.371937394986,0.0145270878443996,
38.4206441795261));
#24334=CARTESIAN_POINT('Ctrl Pts',(-71.3644084675142,0.0124921902170271,
38.3999589890528));
#24335=CARTESIAN_POINT('Ctrl Pts',(-71.324903971772,0.00738822179550698,
38.2925712237683));
#24336=CARTESIAN_POINT('Ctrl Pts',(-71.2979963987338,0.00314156754525118,
38.2182024699665));
#24337=CARTESIAN_POINT('Ctrl Pts',(-71.2648879335367,0.00103199899133368,
38.1267307277737));
#24338=CARTESIAN_POINT('Ctrl Pts',(-71.2459709487275,0.000409937861924508,
38.0738533311077));
#24339=CARTESIAN_POINT('Ctrl Pts',(-71.2433899498565,1.12967778653699E-15,
38.0664089817669));
#24340=CARTESIAN_POINT('Ctrl Pts',(-71.241527913677,1.11022302462517E-15,
38.061269873677));
#24341=CARTESIAN_POINT('Ctrl Pts',(-71.4995507644729,0.0221748194419996,
38.3827594987134));
#24342=CARTESIAN_POINT('Ctrl Pts',(-71.4957111847133,0.0212514804357046,
38.3719446037416));
#24343=CARTESIAN_POINT('Ctrl Pts',(-71.4837469740861,0.0180702925442068,
38.3380317230716));
#24344=CARTESIAN_POINT('Ctrl Pts',(-71.4332256595967,0.0086982168980208,
38.1972090149586));
#24345=CARTESIAN_POINT('Ctrl Pts',(-71.3916700903166,0.0033151901126488,
38.0832652396396));
#24346=CARTESIAN_POINT('Ctrl Pts',(-71.346630963495,0.000434975552779805,
37.9603739181246));
#24347=CARTESIAN_POINT('Ctrl Pts',(-71.3201257651823,-1.2100809912375E-5,
37.8879164256937));
#24348=CARTESIAN_POINT('Ctrl Pts',(-71.3151159005443,5.83926949252806E-16,
37.8741283338393));
#24349=CARTESIAN_POINT('Ctrl Pts',(-71.3125,5.55111512312588E-16,37.8669048105155));
#24350=CARTESIAN_POINT('',(-71.1249759611403,0.0004029778460235,38.5195382755115));
#24351=CARTESIAN_POINT('Ctrl Pts',(-71.099583741031,1.77635683940025E-15,
38.45));
#24352=CARTESIAN_POINT('Ctrl Pts',(-71.0997076102035,1.77661612872688E-15,
38.4503392180609));
#24353=CARTESIAN_POINT('Ctrl Pts',(-71.0998330879728,2.29080306181617E-8,
38.450682841484));
#24354=CARTESIAN_POINT('Ctrl Pts',(-71.0999928315323,1.04590663241311E-7,
38.4511203070689));
#24355=CARTESIAN_POINT('Ctrl Pts',(-71.1001600092189,1.90074632695941E-7,
38.4515781313762));
#24356=CARTESIAN_POINT('Ctrl Pts',(-71.1003645763203,3.3899157853453E-7,
38.4521383523869));
#24357=CARTESIAN_POINT('Ctrl Pts',(-71.1006239759305,6.7627716049401E-7,
38.4528487410268));
#24358=CARTESIAN_POINT('Ctrl Pts',(-71.1009173990762,1.05780200688234E-6,
38.4536523061101));
#24359=CARTESIAN_POINT('Ctrl Pts',(-71.1012809729212,1.68218510490073E-6,
38.4546479901747));
#24360=CARTESIAN_POINT('Ctrl Pts',(-71.1017157284715,2.84078832457624E-6,
38.4558386172851));
#24361=CARTESIAN_POINT('Ctrl Pts',(-71.1021914073984,4.10845043020003E-6,
38.4571413176782));
#24362=CARTESIAN_POINT('Ctrl Pts',(-71.1027518533756,6.03043021784941E-6,
38.4586761669085));
#24363=CARTESIAN_POINT('Ctrl Pts',(-71.1033748256032,8.98260865955791E-6,
38.460382255208));
#24364=CARTESIAN_POINT('Ctrl Pts',(-71.1043065151251,1.33977552724482E-5,
38.4629338048942));
#24365=CARTESIAN_POINT('Ctrl Pts',(-71.105376376433,2.02240544760204E-5,
38.4658637623008));
#24366=CARTESIAN_POINT('Ctrl Pts',(-71.1064700237766,2.96381289164316E-5,
38.4688588618043));
#24367=CARTESIAN_POINT('Ctrl Pts',(-71.1072075567534,3.59867845290267E-5,
38.4708786944914));
#24368=CARTESIAN_POINT('Ctrl Pts',(-71.1079547964485,4.34635710976436E-5,
38.4729251106455));
#24369=CARTESIAN_POINT('Ctrl Pts',(-71.1086850574781,5.17716371906118E-5,
38.4749250268998));
#24370=CARTESIAN_POINT('Ctrl Pts',(-71.1093213961134,5.90111628197922E-5,
38.4766677242757));
#24371=CARTESIAN_POINT('Ctrl Pts',(-71.1099446007745,6.68631518634855E-5,
38.4783744513726));
#24372=CARTESIAN_POINT('Ctrl Pts',(-71.1105507959654,7.51735352766403E-5,
38.4800345929261));
#24373=CARTESIAN_POINT('Ctrl Pts',(-71.1111177706792,8.29462417053621E-5,
38.4815873242844));
#24374=CARTESIAN_POINT('Ctrl Pts',(-71.1116696768522,9.11060770996762E-5,
38.4830987860171));
#24375=CARTESIAN_POINT('Ctrl Pts',(-71.1122192145514,9.97858257232309E-5,
38.4846037563199));
#24376=CARTESIAN_POINT('Ctrl Pts',(-71.1127696572181,0.000108479867978652,
38.4861112049768));
#24377=CARTESIAN_POINT('Ctrl Pts',(-71.113320820801,0.000117743551170355,
38.4876206225949));
#24378=CARTESIAN_POINT('Ctrl Pts',(-71.1138867931674,0.000127862606890794,
38.4891705876114));
#24379=CARTESIAN_POINT('Ctrl Pts',(-71.1144995295096,0.000138817758693007,
38.4908486198817));
#24380=CARTESIAN_POINT('Ctrl Pts',(-71.1151294409423,0.000150785770098267,
38.4925736784895));
#24381=CARTESIAN_POINT('Ctrl Pts',(-71.1157735478178,0.000163820814120363,
38.4943376017864));
#24382=CARTESIAN_POINT('Ctrl Pts',(-71.116526402741,0.000179056635129902,
38.4963993377944));
#24383=CARTESIAN_POINT('Ctrl Pts',(-71.1172983542978,0.000195768933336022,
38.4985133567003));
#24384=CARTESIAN_POINT('Ctrl Pts',(-71.1180605344228,0.000213372206193441,
38.5006006022355));
#24385=CARTESIAN_POINT('Ctrl Pts',(-71.118975496028,0.000234504112240295,
38.5031062429141));
#24386=CARTESIAN_POINT('Ctrl Pts',(-71.119874756806,0.000256914198905863,
38.5055688658886));
#24387=CARTESIAN_POINT('Ctrl Pts',(-71.1206908040971,0.00027844441951963,
38.5078035942042));
#24388=CARTESIAN_POINT('Ctrl Pts',(-71.1213197930097,0.000295039376942754,
38.5095260670908));
#24389=CARTESIAN_POINT('Ctrl Pts',(-71.1218985581243,0.000311061768656351,
38.5111109938185));
#24390=CARTESIAN_POINT('Ctrl Pts',(-71.1224030865798,0.000325452800995052,
38.5124926211035));
#24391=CARTESIAN_POINT('Ctrl Pts',(-71.1228613842659,0.000338525159449124,
38.5137476476155));
#24392=CARTESIAN_POINT('Ctrl Pts',(-71.1232581076796,0.000350230036839969,
38.5148340512162));
#24393=CARTESIAN_POINT('Ctrl Pts',(-71.1235880417374,0.000360129646756135,
38.5157375544699));
#24394=CARTESIAN_POINT('Ctrl Pts',(-71.1238976320008,0.000369418844912552,
38.5165853475476));
#24395=CARTESIAN_POINT('Ctrl Pts',(-71.1241482141858,0.000377107971252698,
38.5172715491176));
#24396=CARTESIAN_POINT('Ctrl Pts',(-71.1243508231998,0.000383380394748833,
38.5178263795026));
#24397=CARTESIAN_POINT('Ctrl Pts',(-71.1245404160348,0.000389249859931833,
38.5183455660067));
#24398=CARTESIAN_POINT('Ctrl Pts',(-71.1246879159046,0.000393876624393683,
38.5187494838655));
#24399=CARTESIAN_POINT('Ctrl Pts',(-71.1248181352022,0.000397984060214185,
38.5191060802768));
#24400=CARTESIAN_POINT('Ctrl Pts',(-71.1248726423429,0.000399703349027781,
38.5192553442575));
#24401=CARTESIAN_POINT('Ctrl Pts',(-71.1249243271121,0.000401338995505559,
38.5193968793866));
#24402=CARTESIAN_POINT('Ctrl Pts',(-71.1249759611403,0.000402977846023944,
38.5195382755115));
#24403=CARTESIAN_POINT('Ctrl Pts',(-71.4995507644729,0.0221748194419996,
38.3827594987134));
#24404=CARTESIAN_POINT('Ctrl Pts',(-71.3746924966954,0.0149175389100076,
38.4283524243128));
#24405=CARTESIAN_POINT('Ctrl Pts',(-71.2498342289178,0.00766025837801554,
38.4739453499121));
#24406=CARTESIAN_POINT('Ctrl Pts',(-71.1249759611403,0.0004029778460235,
38.5195382755115));
#24407=CARTESIAN_POINT('Ctrl Pts',(-71.4995507644729,0.0221748194419993,
38.3827594987134));
#24408=CARTESIAN_POINT('Ctrl Pts',(-71.8031180421414,0.095176430570246,
39.2378135490065));
#24409=CARTESIAN_POINT('Ctrl Pts',(-72.1125000002033,0.389138386673939,
40.2118328742239));
#24410=CARTESIAN_POINT('Ctrl Pts',(-72.1125,0.800000000395795,41.0213168380085));
#24411=CARTESIAN_POINT('Ctrl Pts',(-71.3746924966954,0.0149175389100074,
38.4283524243128));
#24412=CARTESIAN_POINT('Ctrl Pts',(-71.6811443918608,0.0668885519346187,
39.283386933046));
#24413=CARTESIAN_POINT('Ctrl Pts',(-72.0098408305469,0.338541460012493,
40.2544419479763));
#24414=CARTESIAN_POINT('Ctrl Pts',(-72.0395269177012,0.74382707347345,41.0573334705988));
#24415=CARTESIAN_POINT('Ctrl Pts',(-71.2498342289178,0.00766025837801544,
38.4739453499121));
#24416=CARTESIAN_POINT('Ctrl Pts',(-71.5591707415801,0.0386006732989913,
39.3289603170856));
#24417=CARTESIAN_POINT('Ctrl Pts',(-71.9071816608906,0.287944533351047,
40.2970510217287));
#24418=CARTESIAN_POINT('Ctrl Pts',(-71.9665538354024,0.687654146551106,
41.0933501031891));
#24419=CARTESIAN_POINT('Ctrl Pts',(-71.1249759611403,0.0004029778460235,
38.5195382755115));
#24420=CARTESIAN_POINT('Ctrl Pts',(-71.4371970912995,0.010312794663364,
39.3745337011251));
#24421=CARTESIAN_POINT('Ctrl Pts',(-71.8045224912342,0.2373476066896,40.3396600954811));
#24422=CARTESIAN_POINT('Ctrl Pts',(-71.8935807531036,0.631481219628762,
41.1293667357794));
#24423=CARTESIAN_POINT('',(-71.8935807531036,0.631481219628701,41.1293667357793));
#24424=CARTESIAN_POINT('Ctrl Pts',(-71.1249759611403,0.0004029778460235,
38.5195382755115));
#24425=CARTESIAN_POINT('Ctrl Pts',(-71.4371970912995,0.010312794663364,
39.3745337011251));
#24426=CARTESIAN_POINT('Ctrl Pts',(-71.8045224912342,0.2373476066896,40.3396600954811));
#24427=CARTESIAN_POINT('Ctrl Pts',(-71.8935807531036,0.631481219628762,
41.1293667357794));
#24428=CARTESIAN_POINT('',(-71.8935807531036,0.631481219628701,41.1293667357793));
#24429=CARTESIAN_POINT('Origin',(-72.0125,6.00000000000001,38.45));
#24430=CARTESIAN_POINT('',(-71.9125,3.00667409058085,43.65));
#24431=CARTESIAN_POINT('',(-72.1125,3.10645162089482,43.4766666666667));
#24432=CARTESIAN_POINT('',(-71.9125,3.00667409058085,43.65));
#24433=CARTESIAN_POINT('',(-72.1125,0.973333333333333,41.3435483791052));
#24434=CARTESIAN_POINT('Origin',(-72.1125,6.00000000000001,38.45));
#24435=CARTESIAN_POINT('',(-71.9125,0.800000000000003,41.4433259094192));
#24436=CARTESIAN_POINT('',(-72.1125,0.973333333333333,41.3435483791052));
#24437=CARTESIAN_POINT('Origin',(-71.9125,6.00000000000001,38.45));
#24438=CARTESIAN_POINT('Ctrl Pts',(-72.1125,0.80000000039573,41.0213168380084));
#24439=CARTESIAN_POINT('Ctrl Pts',(-72.1125,0.856168534250961,41.1319806866355));
#24440=CARTESIAN_POINT('Ctrl Pts',(-72.1125,0.913326151321779,41.2393040181827));
#24441=CARTESIAN_POINT('Ctrl Pts',(-72.1125,0.973333333333339,41.3435483791052));
#24442=CARTESIAN_POINT('Ctrl Pts',(-72.0395269177012,0.743827073473387,
41.0573334705987));
#24443=CARTESIAN_POINT('Ctrl Pts',(-72.0435852768747,0.799233317184012,
41.1670960723289));
#24444=CARTESIAN_POINT('Ctrl Pts',(-72.0458333333333,0.85614614623837,41.2736016445264));
#24445=CARTESIAN_POINT('Ctrl Pts',(-72.0458333333333,0.915555555555561,
41.3768075558765));
#24446=CARTESIAN_POINT('Ctrl Pts',(-71.9665538354024,0.687654146551043,
41.093350103189));
#24447=CARTESIAN_POINT('Ctrl Pts',(-71.9746705537493,0.742298100117063,
41.2022114580222));
#24448=CARTESIAN_POINT('Ctrl Pts',(-71.9791666666667,0.798966141154961,
41.3078992708702));
#24449=CARTESIAN_POINT('Ctrl Pts',(-71.9791666666667,0.857777777777783,
41.4100667326478));
#24450=CARTESIAN_POINT('Ctrl Pts',(-71.8935807531036,0.631481219628699,
41.1293667357793));
#24451=CARTESIAN_POINT('Ctrl Pts',(-71.905755830624,0.685362883050115,41.2373268437155));
#24452=CARTESIAN_POINT('Ctrl Pts',(-71.9125,0.741786136071552,41.3421968972139));
#24453=CARTESIAN_POINT('Ctrl Pts',(-71.9125,0.800000000000005,41.4433259094192));
#24454=CARTESIAN_POINT('Ctrl Pts',(-72.1125,0.973333333333339,41.3435483791052));
#24455=CARTESIAN_POINT('Ctrl Pts',(-72.1125,0.913326151321779,41.2393040181827));
#24456=CARTESIAN_POINT('Ctrl Pts',(-72.1125,0.856168534250961,41.1319806866355));
#24457=CARTESIAN_POINT('Ctrl Pts',(-72.1125,0.80000000039573,41.0213168380084));
#24458=CARTESIAN_POINT('Ctrl Pts',(-71.8935807531036,0.631481219628699,
41.1293667357793));
#24459=CARTESIAN_POINT('Ctrl Pts',(-71.905755830624,0.685362883050115,41.2373268437155));
#24460=CARTESIAN_POINT('Ctrl Pts',(-71.9125,0.741786136071552,41.3421968972139));
#24461=CARTESIAN_POINT('Ctrl Pts',(-71.9125,0.800000000000005,41.4433259094192));
#24462=CARTESIAN_POINT('Ctrl Pts',(-72.1125,3.42868316199152,43.6499999996042));
#24463=CARTESIAN_POINT('Ctrl Pts',(-72.1125000002033,4.23816756991044,44.0608618387509));
#24464=CARTESIAN_POINT('Ctrl Pts',(-71.8031170174309,5.21218945423946,44.3548240219809));
#24465=CARTESIAN_POINT('Ctrl Pts',(-71.4995502651833,6.0672419076457,44.4278253006266));
#24466=CARTESIAN_POINT('Ctrl Pts',(-72.0395269177012,3.3926665294012,43.7061729265265));
#24467=CARTESIAN_POINT('Ctrl Pts',(-72.0098408142592,4.19555849254101,44.111458762353));
#24468=CARTESIAN_POINT('Ctrl Pts',(-71.6811438122403,5.16661477993893,44.3831118133254));
#24469=CARTESIAN_POINT('Ctrl Pts',(-71.3746919924044,6.0216489827177,44.4350825465769));
#24470=CARTESIAN_POINT('Ctrl Pts',(-71.9665538354024,3.35664989681089,43.7623458534489));
#24471=CARTESIAN_POINT('Ctrl Pts',(-71.9071816283152,4.15294941517159,44.1620556859551));
#24472=CARTESIAN_POINT('Ctrl Pts',(-71.5591706070498,5.12104010563839,44.4113996046699));
#24473=CARTESIAN_POINT('Ctrl Pts',(-71.2498337196255,5.9760560577897,44.4423397925272));
#24474=CARTESIAN_POINT('Ctrl Pts',(-71.8935807531036,3.32063326422057,43.8185187803712));
#24475=CARTESIAN_POINT('Ctrl Pts',(-71.8045224423712,4.11034033780217,44.2126526095572));
#24476=CARTESIAN_POINT('Ctrl Pts',(-71.4371974018592,5.07546543133786,44.4396873960144));
#24477=CARTESIAN_POINT('Ctrl Pts',(-71.1249754468465,5.93046313286171,44.4495970384775));
#24478=CARTESIAN_POINT('',(-72.1125,3.42868316190267,43.6499999997796));
#24479=CARTESIAN_POINT('Ctrl Pts',(-71.4995502651833,6.0672419076457,44.4278253006266));
#24480=CARTESIAN_POINT('Ctrl Pts',(-71.8031170174309,5.21218945423946,44.3548240219809));
#24481=CARTESIAN_POINT('Ctrl Pts',(-72.1125000002033,4.23816756991044,44.0608618387509));
#24482=CARTESIAN_POINT('Ctrl Pts',(-72.1125,3.42868316199152,43.6499999996042));
#24483=CARTESIAN_POINT('',(-71.8935807531036,3.32063326422069,43.8185187803713));
#24484=CARTESIAN_POINT('',(-72.1125,3.42868316190267,43.6499999997796));
#24485=CARTESIAN_POINT('Ctrl Pts',(-71.8935807531036,3.32063326422057,43.8185187803712));
#24486=CARTESIAN_POINT('Ctrl Pts',(-71.8045224423712,4.11034033780217,44.2126526095572));
#24487=CARTESIAN_POINT('Ctrl Pts',(-71.4371974018592,5.07546543133786,44.4396873960144));
#24488=CARTESIAN_POINT('Ctrl Pts',(-71.1249754468465,5.93046313286171,44.4495970384775));
#24489=CARTESIAN_POINT('Ctrl Pts',(-72.1125,3.10645162089483,43.4766666666667));
#24490=CARTESIAN_POINT('Ctrl Pts',(-72.1125,3.2106959818173,43.5366738486782));
#24491=CARTESIAN_POINT('Ctrl Pts',(-72.1125,3.31801931336448,43.593831465749));
#24492=CARTESIAN_POINT('Ctrl Pts',(-72.1125,3.42868316199164,43.6499999996043));
#24493=CARTESIAN_POINT('Ctrl Pts',(-72.0458333333333,3.0731924441235,43.5344444444444));
#24494=CARTESIAN_POINT('Ctrl Pts',(-72.0458333333333,3.17639835547357,43.5938538537616));
#24495=CARTESIAN_POINT('Ctrl Pts',(-72.0435852768747,3.28290392767114,43.650766682816));
#24496=CARTESIAN_POINT('Ctrl Pts',(-72.0395269177012,3.39266652940132,43.7061729265266));
#24497=CARTESIAN_POINT('Ctrl Pts',(-71.9791666666667,3.03993326735218,43.5922222222222));
#24498=CARTESIAN_POINT('Ctrl Pts',(-71.9791666666667,3.14210072912984,43.651033858845));
#24499=CARTESIAN_POINT('Ctrl Pts',(-71.9746705537493,3.2477885419778,43.7077018998829));
#24500=CARTESIAN_POINT('Ctrl Pts',(-71.9665538354024,3.35664989681101,43.762345853449));
#24501=CARTESIAN_POINT('Ctrl Pts',(-71.9125,3.00667409058085,43.65));
#24502=CARTESIAN_POINT('Ctrl Pts',(-71.9125,3.1078031027861,43.7082138639284));
#24503=CARTESIAN_POINT('Ctrl Pts',(-71.905755830624,3.21267315628445,43.7646371169499));
#24504=CARTESIAN_POINT('Ctrl Pts',(-71.8935807531036,3.32063326422069,43.8185187803713));
#24505=CARTESIAN_POINT('Ctrl Pts',(-72.1125,3.42868316199164,43.6499999996043));
#24506=CARTESIAN_POINT('Ctrl Pts',(-72.1125,3.31801931336448,43.593831465749));
#24507=CARTESIAN_POINT('Ctrl Pts',(-72.1125,3.2106959818173,43.5366738486782));
#24508=CARTESIAN_POINT('Ctrl Pts',(-72.1125,3.10645162089483,43.4766666666667));
#24509=CARTESIAN_POINT('Ctrl Pts',(-71.9125,3.00667409058085,43.65));
#24510=CARTESIAN_POINT('Ctrl Pts',(-71.9125,3.1078031027861,43.7082138639284));
#24511=CARTESIAN_POINT('Ctrl Pts',(-71.905755830624,3.21267315628445,43.7646371169499));
#24512=CARTESIAN_POINT('Ctrl Pts',(-71.8935807531036,3.32063326422069,43.8185187803713));
#24513=CARTESIAN_POINT('Origin',(-72.1125,63.5,-31.75));
#24514=CARTESIAN_POINT('',(-72.1125,123.993325909419,43.65));
#24515=CARTESIAN_POINT('',(-72.1125,34.75,43.65));
#24516=CARTESIAN_POINT('',(-72.1125,126.2,41.4433259094192));
#24517=CARTESIAN_POINT('Origin',(-72.1125,121.,38.45));
#24518=CARTESIAN_POINT('',(-72.1125,126.2,-104.943325909419));
#24519=CARTESIAN_POINT('',(-72.1125,126.2,3.35000000000001));
#24520=CARTESIAN_POINT('',(-72.1125,123.993325909419,-107.15));
#24521=CARTESIAN_POINT('Origin',(-72.1125,121.,-101.95));
#24522=CARTESIAN_POINT('',(-72.1125,92.25,-107.15));
#24523=CARTESIAN_POINT('Origin',(-67.35,6.00000000000001,38.45));
#24524=CARTESIAN_POINT('Origin',(-68.15,0.800000000000001,-66.85));
#24525=CARTESIAN_POINT('Origin',(-71.3125,34.75,43.65));
#24526=CARTESIAN_POINT('Ctrl Pts',(-71.3125,121.,44.45));
#24527=CARTESIAN_POINT('Ctrl Pts',(-71.4899908431149,121.486078692623,44.45));
#24528=CARTESIAN_POINT('Ctrl Pts',(-71.6844866658569,122.014025751789,44.387608349819));
#24529=CARTESIAN_POINT('Ctrl Pts',(-71.9943880775948,123.043713064318,44.1162803662604));
#24530=CARTESIAN_POINT('Ctrl Pts',(-72.1125,123.544851663295,43.9081595347366));
#24531=CARTESIAN_POINT('Ctrl Pts',(-72.1125,123.993325909419,43.65));
#24532=CARTESIAN_POINT('Origin',(-67.35,121.,38.45));
#24533=CARTESIAN_POINT('',(-68.15,127.,38.45));
#24534=CARTESIAN_POINT('Ctrl Pts',(-68.15,127.,38.45));
#24535=CARTESIAN_POINT('Ctrl Pts',(-67.9725091568851,127.,38.9360786926232));
#24536=CARTESIAN_POINT('Ctrl Pts',(-67.7780133341431,126.937608349819,39.4640257517887));
#24537=CARTESIAN_POINT('Ctrl Pts',(-67.4681119224052,126.66628036626,40.4937130643181));
#24538=CARTESIAN_POINT('Ctrl Pts',(-67.35,126.458159534737,40.9948516632952));
#24539=CARTESIAN_POINT('Ctrl Pts',(-67.35,126.2,41.4433259094192));
#24540=CARTESIAN_POINT('',(-71.3125,127.,38.45));
#24541=CARTESIAN_POINT('',(-67.35,127.,38.45));
#24542=CARTESIAN_POINT('Ctrl Pts',(-72.1125,126.2,41.4433259094192));
#24543=CARTESIAN_POINT('Ctrl Pts',(-72.1125,126.458159534737,40.9948516632952));
#24544=CARTESIAN_POINT('Ctrl Pts',(-71.9943880775948,126.66628036626,40.4937130643181));
#24545=CARTESIAN_POINT('Ctrl Pts',(-71.6844866658569,126.937608349819,39.4640257517887));
#24546=CARTESIAN_POINT('Ctrl Pts',(-71.4899908431149,127.,38.9360786926232));
#24547=CARTESIAN_POINT('Ctrl Pts',(-71.3125,127.,38.45));
#24548=CARTESIAN_POINT('Origin',(-71.3125,126.2,3.35000000000001));
#24549=CARTESIAN_POINT('',(-71.3125,127.,-101.95));
#24550=CARTESIAN_POINT('Ctrl Pts',(-71.3125,127.,-101.95));
#24551=CARTESIAN_POINT('Ctrl Pts',(-71.4899908431149,127.,-102.436078692623));
#24552=CARTESIAN_POINT('Ctrl Pts',(-71.6844866658568,126.937608349819,-102.964025751789));
#24553=CARTESIAN_POINT('Ctrl Pts',(-71.9943880775948,126.66628036626,-103.993713064318));
#24554=CARTESIAN_POINT('Ctrl Pts',(-72.1125,126.458159534737,-104.494851663295));
#24555=CARTESIAN_POINT('Ctrl Pts',(-72.1125,126.2,-104.943325909419));
#24556=CARTESIAN_POINT('',(-71.3125,127.,3.35000000000001));
#24557=CARTESIAN_POINT('Origin',(-67.35,121.,-101.95));
#24558=CARTESIAN_POINT('',(-68.15,127.,-101.95));
#24559=CARTESIAN_POINT('',(-67.35,127.,-101.95));
#24560=CARTESIAN_POINT('Ctrl Pts',(-67.35,126.2,-104.943325909419));
#24561=CARTESIAN_POINT('Ctrl Pts',(-67.35,126.458159534737,-104.494851663295));
#24562=CARTESIAN_POINT('Ctrl Pts',(-67.4681119224052,126.66628036626,-103.993713064318));
#24563=CARTESIAN_POINT('Ctrl Pts',(-67.7780133341432,126.937608349819,-102.964025751789));
#24564=CARTESIAN_POINT('Ctrl Pts',(-67.9725091568851,127.,-102.436078692623));
#24565=CARTESIAN_POINT('Ctrl Pts',(-68.15,127.,-101.95));
#24566=CARTESIAN_POINT('Ctrl Pts',(-72.1125,123.993325909419,-107.15));
#24567=CARTESIAN_POINT('Ctrl Pts',(-72.1125,123.544851663295,-107.408159534737));
#24568=CARTESIAN_POINT('Ctrl Pts',(-71.9943880775948,123.043713064318,-107.61628036626));
#24569=CARTESIAN_POINT('Ctrl Pts',(-71.6844866658569,122.014025751789,-107.887608349819));
#24570=CARTESIAN_POINT('Ctrl Pts',(-71.4899908431149,121.486078692623,-107.95));
#24571=CARTESIAN_POINT('Ctrl Pts',(-71.3125,121.,-107.95));
#24572=CARTESIAN_POINT('Origin',(-67.35,127.,38.45));
#24573=CARTESIAN_POINT('',(-68.15,127.,3.35000000000001));
#24574=CARTESIAN_POINT('Origin',(-68.15,126.2,3.35000000000001));
#24575=CARTESIAN_POINT('Origin',(-71.3125,92.25,-107.15));
#24576=CARTESIAN_POINT('',(0.,0.,0.));
#24577=CARTESIAN_POINT('Ctrl Pts',(-66.2975371703006,122.238070190751,43.6801990080023));
#24578=CARTESIAN_POINT('Ctrl Pts',(-66.295869694655,122.238006634921,43.678516554556));
#24579=CARTESIAN_POINT('Ctrl Pts',(-66.2836640413214,122.237567815036,43.6661713539299));
#24580=CARTESIAN_POINT('Ctrl Pts',(-66.2702842984222,122.237504067589,43.6526075471718));
#24581=CARTESIAN_POINT('Ctrl Pts',(-66.2681224083043,122.2375,43.6504214071384));
#24582=CARTESIAN_POINT('Ctrl Pts',(-66.2677059397486,122.2375,43.65));
#24583=CARTESIAN_POINT('Ctrl Pts',(-66.3917577828678,122.238070190751,43.5859783954351));
#24584=CARTESIAN_POINT('Ctrl Pts',(-66.390085314622,122.238006634921,43.584300934589));
#24585=CARTESIAN_POINT('Ctrl Pts',(-66.3778263299278,122.237567815036,43.5720090653235));
#24586=CARTESIAN_POINT('Ctrl Pts',(-66.3643944630001,122.237504067589,43.558497382594));
#24587=CARTESIAN_POINT('Ctrl Pts',(-66.3622220745824,122.2375,43.5563217408604));
#24588=CARTESIAN_POINT('Ctrl Pts',(-66.3618039598324,122.2375,43.5559019799162));
#24589=CARTESIAN_POINT('Ctrl Pts',(-66.4859783954351,122.238070190751,43.4917577828678));
#24590=CARTESIAN_POINT('Ctrl Pts',(-66.484300934589,122.238006634921,43.490085314622));
#24591=CARTESIAN_POINT('Ctrl Pts',(-66.4719682708158,122.237492703884,43.4778263299279));
#24592=CARTESIAN_POINT('Ctrl Pts',(-66.4584917270448,122.23754961255,43.464394463));
#24593=CARTESIAN_POINT('Ctrl Pts',(-66.4563217408604,122.2375,43.4622220745823));
#24594=CARTESIAN_POINT('Ctrl Pts',(-66.4559019799162,122.2375,43.4618039598323));
#24595=CARTESIAN_POINT('Ctrl Pts',(-66.5801990080023,122.238070190751,43.3975371703006));
#24596=CARTESIAN_POINT('Ctrl Pts',(-66.578516554556,122.238006634921,43.395869694655));
#24597=CARTESIAN_POINT('Ctrl Pts',(-66.5661713539299,122.237567815036,43.3836640413215));
#24598=CARTESIAN_POINT('Ctrl Pts',(-66.5526075471718,122.237504067589,43.3702842984222));
#24599=CARTESIAN_POINT('Ctrl Pts',(-66.5504214071384,122.2375,43.3681224083043));
#24600=CARTESIAN_POINT('Ctrl Pts',(-66.55,122.2375,43.3677059397485));
#24601=CARTESIAN_POINT('',(-66.2677059397486,122.2375,43.65));
#24602=CARTESIAN_POINT('',(-66.2975371703006,122.238070190751,43.6801990080023));
#24603=CARTESIAN_POINT('Ctrl Pts',(-66.2677059397486,122.2375,43.65));
#24604=CARTESIAN_POINT('Ctrl Pts',(-66.2678726988052,122.2375,43.650168736525));
#24605=CARTESIAN_POINT('Ctrl Pts',(-66.2680426727623,122.237500039141,43.6503407294752));
#24606=CARTESIAN_POINT('Ctrl Pts',(-66.2682711198522,122.237500204467,43.6505719684178));
#24607=CARTESIAN_POINT('Ctrl Pts',(-66.2685232393849,122.237500386926,43.6508271691041));
#24608=CARTESIAN_POINT('Ctrl Pts',(-66.2688465074852,122.23750071898,43.6511544591101));
#24609=CARTESIAN_POINT('Ctrl Pts',(-66.2692682628933,122.237501563317,43.6515815512717));
#24610=CARTESIAN_POINT('Ctrl Pts',(-66.2697392792016,122.237502506272,43.6520585276647));
#24611=CARTESIAN_POINT('Ctrl Pts',(-66.2703326618206,122.237504104656,43.6526595049514));
#24612=CARTESIAN_POINT('Ctrl Pts',(-66.2710345962128,122.237507100231,43.6533705073353));
#24613=CARTESIAN_POINT('Ctrl Pts',(-66.271922356591,122.237510888837,43.6542697363121));
#24614=CARTESIAN_POINT('Ctrl Pts',(-66.2729823430601,122.237517016609,43.6553435322326));
#24615=CARTESIAN_POINT('Ctrl Pts',(-66.274119373636,122.237526369906,43.6564954718404));
#24616=CARTESIAN_POINT('Ctrl Pts',(-66.275267024347,122.237535810566,43.6576581708371));
#24617=CARTESIAN_POINT('Ctrl Pts',(-66.2764877640867,122.237548536479,43.6588950097937));
#24618=CARTESIAN_POINT('Ctrl Pts',(-66.2776823234139,122.237563826519,43.6601053627627));
#24619=CARTESIAN_POINT('Ctrl Pts',(-66.2785768692241,122.237575276466,43.6610117356425));
#24620=CARTESIAN_POINT('Ctrl Pts',(-66.2794562057464,122.237588088159,43.6619027203554));
#24621=CARTESIAN_POINT('Ctrl Pts',(-66.2803059516487,122.237601826337,43.6627636895375));
#24622=CARTESIAN_POINT('Ctrl Pts',(-66.2810774585305,122.237614299594,43.6635453863334));
#24623=CARTESIAN_POINT('Ctrl Pts',(-66.2818241823993,122.237627497267,43.6643019452828));
#24624=CARTESIAN_POINT('Ctrl Pts',(-66.2825668820939,122.237641657879,43.6650543196431));
#24625=CARTESIAN_POINT('Ctrl Pts',(-66.2833438316762,122.237656471514,43.6658413900423));
#24626=CARTESIAN_POINT('Ctrl Pts',(-66.2841235557123,122.23767247258,43.6666311424701));
#24627=CARTESIAN_POINT('Ctrl Pts',(-66.2849308055329,122.237690305677,43.6674485777765));
#24628=CARTESIAN_POINT('Ctrl Pts',(-66.2858320241453,122.237710214654,43.6683611675274));
#24629=CARTESIAN_POINT('Ctrl Pts',(-66.286766994243,122.237732447118,43.6693076969554));
#24630=CARTESIAN_POINT('Ctrl Pts',(-66.2877173601371,122.237756826022,43.6702695751379));
#24631=CARTESIAN_POINT('Ctrl Pts',(-66.2889597634694,122.237788696307,43.6715270283639));
#24632=CARTESIAN_POINT('Ctrl Pts',(-66.2902267818597,122.237824333785,43.6728089911267));
#24633=CARTESIAN_POINT('Ctrl Pts',(-66.2914048119203,122.237860099073,43.6740006009414));
#24634=CARTESIAN_POINT('Ctrl Pts',(-66.2923675692485,122.237889328627,43.6749744564649));
#24635=CARTESIAN_POINT('Ctrl Pts',(-66.293267661289,122.237918483816,43.6758847018469));
#24636=CARTESIAN_POINT('Ctrl Pts',(-66.2940452683694,122.237944709538,43.6766709110186));
#24637=CARTESIAN_POINT('Ctrl Pts',(-66.2947223806606,122.237967545954,43.6773555137016));
#24638=CARTESIAN_POINT('Ctrl Pts',(-66.2953057241463,122.237988087761,43.6779451634303));
#24639=CARTESIAN_POINT('Ctrl Pts',(-66.295779966785,122.238005126535,43.6784244138564));
#24640=CARTESIAN_POINT('Ctrl Pts',(-66.2962183038067,122.238020875278,43.6788673795184));
#24641=CARTESIAN_POINT('Ctrl Pts',(-66.2965629424176,122.238033598544,43.679215532934));
#24642=CARTESIAN_POINT('Ctrl Pts',(-66.2968329073597,122.238043654136,43.6794881511418));
#24643=CARTESIAN_POINT('Ctrl Pts',(-66.2970837268897,122.238052996604,43.6797414357728));
#24644=CARTESIAN_POINT('Ctrl Pts',(-66.297269873309,122.238060029675,43.6799293013871));
#24645=CARTESIAN_POINT('Ctrl Pts',(-66.297439207674,122.238066462969,43.6801001639575));
#24646=CARTESIAN_POINT('Ctrl Pts',(-66.2974722152538,122.238067716982,43.6801334694236));
#24647=CARTESIAN_POINT('Ctrl Pts',(-66.2975046952455,122.238068952964,43.6801662412459));
#24648=CARTESIAN_POINT('Ctrl Pts',(-66.2975371703006,122.238070190751,43.6801990080023));
#24649=CARTESIAN_POINT('',(-66.5801990080023,122.238070190751,43.3975371703006));
#24650=CARTESIAN_POINT('Ctrl Pts',(-66.5801990080023,122.238070190751,43.3975371703006));
#24651=CARTESIAN_POINT('Ctrl Pts',(-66.4859783954351,122.238070190751,43.4917577828678));
#24652=CARTESIAN_POINT('Ctrl Pts',(-66.3917577828678,122.238070190751,43.5859783954351));
#24653=CARTESIAN_POINT('Ctrl Pts',(-66.2975371703006,122.238070190751,43.6801990080023));
#24654=CARTESIAN_POINT('',(-66.55,122.2375,43.3677059397485));
#24655=CARTESIAN_POINT('Ctrl Pts',(-66.5801990080023,122.238070190751,43.3975371703006));
#24656=CARTESIAN_POINT('Ctrl Pts',(-66.5800305855052,122.238063828476,43.3973702471606));
#24657=CARTESIAN_POINT('Ctrl Pts',(-66.5798589093858,122.238057382362,43.397200107149));
#24658=CARTESIAN_POINT('Ctrl Pts',(-66.579628057339,122.23804882687,43.3969714633112));
#24659=CARTESIAN_POINT('Ctrl Pts',(-66.579373282892,122.238039384803,43.3967191259023));
#24660=CARTESIAN_POINT('Ctrl Pts',(-66.579046504163,122.238027372131,43.3963956021263));
#24661=CARTESIAN_POINT('Ctrl Pts',(-66.5786200261656,122.238012105093,43.3959735434092));
#24662=CARTESIAN_POINT('Ctrl Pts',(-66.5781437326004,122.237995054761,43.3955021853267));
#24663=CARTESIAN_POINT('Ctrl Pts',(-66.5775435637608,122.237973979824,43.3949084001561));
#24664=CARTESIAN_POINT('Ctrl Pts',(-66.5768334404113,122.237950147598,43.3942060222412));
#24665=CARTESIAN_POINT('Ctrl Pts',(-66.5759352908255,122.237920005083,43.3933176689237));
#24666=CARTESIAN_POINT('Ctrl Pts',(-66.5748626695,122.237885609635,43.3922570121513));
#24667=CARTESIAN_POINT('Ctrl Pts',(-66.5737118227387,122.237851483799,43.3911193310077));
#24668=CARTESIAN_POINT('Ctrl Pts',(-66.5725503239299,122.2378170421,43.3899711196752));
#24669=CARTESIAN_POINT('Ctrl Pts',(-66.5713146082228,122.237783080562,43.3887498553891));
#24670=CARTESIAN_POINT('Ctrl Pts',(-66.5701051310901,122.237752675088,43.3875548864531));
#24671=CARTESIAN_POINT('Ctrl Pts',(-66.5691994017694,122.237729905638,43.3866600217438));
#24672=CARTESIAN_POINT('Ctrl Pts',(-66.5683089239631,122.237709074602,43.3857804315059));
#24673=CARTESIAN_POINT('Ctrl Pts',(-66.5674482886096,122.237690299368,43.3849305199691));
#24674=CARTESIAN_POINT('Ctrl Pts',(-66.5666668879855,122.237673252684,43.3841588558693));
#24675=CARTESIAN_POINT('Ctrl Pts',(-66.5659104838912,122.237657876347,43.3834120480763));
#24676=CARTESIAN_POINT('Ctrl Pts',(-66.5651581113835,122.237643618104,43.3826693398989));
#24677=CARTESIAN_POINT('Ctrl Pts',(-66.5643710534174,122.237628702536,43.3818923918027));
#24678=CARTESIAN_POINT('Ctrl Pts',(-66.5635811455704,122.237614869895,43.3811127516152));
#24679=CARTESIAN_POINT('Ctrl Pts',(-66.5627634000951,122.237601821718,43.3803056659794));
#24680=CARTESIAN_POINT('Ctrl Pts',(-66.5618504525924,122.237587254472,43.3794046193358));
#24681=CARTESIAN_POINT('Ctrl Pts',(-66.5609033701718,122.237573726381,43.378469920108));
#24682=CARTESIAN_POINT('Ctrl Pts',(-66.5599407885337,122.237561764432,43.377519896467));
#24683=CARTESIAN_POINT('Ctrl Pts',(-66.5586823476285,122.237546125856,43.3762778733873));
#24684=CARTESIAN_POINT('Ctrl Pts',(-66.5573991342584,122.237533328235,43.3750113535098));
#24685=CARTESIAN_POINT('Ctrl Pts',(-66.5562062234238,122.237524073618,43.3738338670347));
#24686=CARTESIAN_POINT('Ctrl Pts',(-66.555231427366,122.237516511138,43.3728716751083));
#24687=CARTESIAN_POINT('Ctrl Pts',(-66.5543201973287,122.237511277906,43.3719721616152));
#24688=CARTESIAN_POINT('Ctrl Pts',(-66.5535330697621,122.237507801652,43.3711950841759));
#24689=CARTESIAN_POINT('Ctrl Pts',(-66.5528476493566,122.237504774575,43.37051841529));
#24690=CARTESIAN_POINT('Ctrl Pts',(-66.5522572394504,122.237503040519,43.3699354824523));
#24691=CARTESIAN_POINT('Ctrl Pts',(-66.5517773349746,122.237501974327,43.3694615957548));
#24692=CARTESIAN_POINT('Ctrl Pts',(-66.5513337613121,122.237500988851,43.369023584299));
#24693=CARTESIAN_POINT('Ctrl Pts',(-66.5509850931076,122.237500559908,43.3686792256942));
#24694=CARTESIAN_POINT('Ctrl Pts',(-66.5507120440952,122.237500316879,43.3684094978756));
#24695=CARTESIAN_POINT('Ctrl Pts',(-66.5504583577137,122.237500091084,43.3681588971731));
#24696=CARTESIAN_POINT('Ctrl Pts',(-66.5502701637948,122.237500027304,43.3679729332267));
#24697=CARTESIAN_POINT('Ctrl Pts',(-66.5500989877785,122.237500006124,43.3678037667746));
#24698=CARTESIAN_POINT('Ctrl Pts',(-66.5500656344477,122.237500001997,43.3677708050036));
#24699=CARTESIAN_POINT('Ctrl Pts',(-66.5500328147292,122.2375,43.3677383699132));
#24700=CARTESIAN_POINT('Ctrl Pts',(-66.55,122.2375,43.3677059397485));
#24701=CARTESIAN_POINT('',(-66.4088529698743,122.2375,43.5088529698743));
#24702=CARTESIAN_POINT('Ctrl Pts',(-66.5801990080023,126.999429809249,43.3975371703006));
#24703=CARTESIAN_POINT('Ctrl Pts',(-66.578516554556,126.999493365079,43.395869694655));
#24704=CARTESIAN_POINT('Ctrl Pts',(-66.5661715453635,126.999932181252,43.383664231718));
#24705=CARTESIAN_POINT('Ctrl Pts',(-66.5526075968239,126.999995931781,43.3702843477267));
#24706=CARTESIAN_POINT('Ctrl Pts',(-66.5504214071384,127.,43.3681224083043));
#24707=CARTESIAN_POINT('Ctrl Pts',(-66.55,127.,43.3677059397485));
#24708=CARTESIAN_POINT('Ctrl Pts',(-66.4859783954351,126.999429809249,43.4917577828678));
#24709=CARTESIAN_POINT('Ctrl Pts',(-66.484300934589,126.999493365079,43.490085314622));
#24710=CARTESIAN_POINT('Ctrl Pts',(-66.4720092567571,126.999932181252,43.4778265203243));
#24711=CARTESIAN_POINT('Ctrl Pts',(-66.458497432246,126.999995931781,43.4643945123045));
#24712=CARTESIAN_POINT('Ctrl Pts',(-66.4563217408604,127.,43.4622220745824));
#24713=CARTESIAN_POINT('Ctrl Pts',(-66.4559019799162,127.,43.4618039598323));
#24714=CARTESIAN_POINT('Ctrl Pts',(-66.3917577828678,126.999429809249,43.5859783954351));
#24715=CARTESIAN_POINT('Ctrl Pts',(-66.390085314622,126.999493365079,43.584300934589));
#24716=CARTESIAN_POINT('Ctrl Pts',(-66.3778265203244,127.000007314886,43.5719684631258));
#24717=CARTESIAN_POINT('Ctrl Pts',(-66.3643945123046,126.999950392654,43.5584917768456));
#24718=CARTESIAN_POINT('Ctrl Pts',(-66.3622220745824,127.,43.5563217408604));
#24719=CARTESIAN_POINT('Ctrl Pts',(-66.3618039598324,127.,43.5559019799162));
#24720=CARTESIAN_POINT('Ctrl Pts',(-66.2975371703006,126.999429809249,43.6801990080023));
#24721=CARTESIAN_POINT('Ctrl Pts',(-66.295869694655,126.999493365079,43.678516554556));
#24722=CARTESIAN_POINT('Ctrl Pts',(-66.283664231718,126.999932181252,43.6661715453635));
#24723=CARTESIAN_POINT('Ctrl Pts',(-66.2702843477267,126.999995931781,43.6526075968239));
#24724=CARTESIAN_POINT('Ctrl Pts',(-66.2681224083043,127.,43.6504214071384));
#24725=CARTESIAN_POINT('Ctrl Pts',(-66.2677059397486,127.,43.65));
#24726=CARTESIAN_POINT('',(-66.55,127.,43.3677059397485));
#24727=CARTESIAN_POINT('',(-66.5801990080023,126.999429809249,43.3975371703006));
#24728=CARTESIAN_POINT('Ctrl Pts',(-66.55,127.,43.3677059397485));
#24729=CARTESIAN_POINT('Ctrl Pts',(-66.550168736525,127.,43.3678726988052));
#24730=CARTESIAN_POINT('Ctrl Pts',(-66.5503407294752,126.999999960859,43.3680426727623));
#24731=CARTESIAN_POINT('Ctrl Pts',(-66.5505719684178,126.999999795533,43.3682711198522));
#24732=CARTESIAN_POINT('Ctrl Pts',(-66.5508271691041,126.999999613074,43.3685232393849));
#24733=CARTESIAN_POINT('Ctrl Pts',(-66.5511544591101,126.99999928102,43.3688465074852));
#24734=CARTESIAN_POINT('Ctrl Pts',(-66.5515815512717,126.999998436683,43.3692682628933));
#24735=CARTESIAN_POINT('Ctrl Pts',(-66.5520585276647,126.999997493728,43.3697392792016));
#24736=CARTESIAN_POINT('Ctrl Pts',(-66.5526595049514,126.999995895344,43.3703326618206));
#24737=CARTESIAN_POINT('Ctrl Pts',(-66.5533705073353,126.999992899769,43.3710345962128));
#24738=CARTESIAN_POINT('Ctrl Pts',(-66.554269736312,126.999989111163,43.371922356591));
#24739=CARTESIAN_POINT('Ctrl Pts',(-66.5553435322326,126.999982983391,43.37298234306));
#24740=CARTESIAN_POINT('Ctrl Pts',(-66.5564954718403,126.999973630094,43.3741193736359));
#24741=CARTESIAN_POINT('Ctrl Pts',(-66.5576581708369,126.999964189434,43.3752670243469));
#24742=CARTESIAN_POINT('Ctrl Pts',(-66.5588950097936,126.999951463521,43.3764877640866));
#24743=CARTESIAN_POINT('Ctrl Pts',(-66.5601053627626,126.999936173481,43.3776823234138));
#24744=CARTESIAN_POINT('Ctrl Pts',(-66.5610117356423,126.999924723534,43.378576869224));
#24745=CARTESIAN_POINT('Ctrl Pts',(-66.5619027203552,126.999911911841,43.3794562057463));
#24746=CARTESIAN_POINT('Ctrl Pts',(-66.5627636895374,126.999898173663,43.3803059516486));
#24747=CARTESIAN_POINT('Ctrl Pts',(-66.5635453863323,126.999885700406,43.3810774585295));
#24748=CARTESIAN_POINT('Ctrl Pts',(-66.5643019452809,126.999872502733,43.3818241823974));
#24749=CARTESIAN_POINT('Ctrl Pts',(-66.5650543196403,126.999858342121,43.3825668820911));
#24750=CARTESIAN_POINT('Ctrl Pts',(-66.5658413900395,126.999843528486,43.3833438316734));
#24751=CARTESIAN_POINT('Ctrl Pts',(-66.5666311424671,126.99982752742,43.3841235557094));
#24752=CARTESIAN_POINT('Ctrl Pts',(-66.5674485777734,126.999809694323,43.3849308055298));
#24753=CARTESIAN_POINT('Ctrl Pts',(-66.5683611675241,126.999789785346,43.385832024142));
#24754=CARTESIAN_POINT('Ctrl Pts',(-66.5693076969518,126.999767552882,43.3867669942395));
#24755=CARTESIAN_POINT('Ctrl Pts',(-66.5702695751342,126.999743173978,43.3877173601334));
#24756=CARTESIAN_POINT('Ctrl Pts',(-66.5715270283595,126.999711303693,43.3889597634651));
#24757=CARTESIAN_POINT('Ctrl Pts',(-66.5728089911216,126.999675666215,43.3902267818547));
#24758=CARTESIAN_POINT('Ctrl Pts',(-66.5740006009359,126.999639900927,43.3914048119149));
#24759=CARTESIAN_POINT('Ctrl Pts',(-66.57497445646,126.999610671373,43.3923675692436));
#24760=CARTESIAN_POINT('Ctrl Pts',(-66.5758847018426,126.999581516184,43.3932676612848));
#24761=CARTESIAN_POINT('Ctrl Pts',(-66.5766709110149,126.999555290462,43.3940452683658));
#24762=CARTESIAN_POINT('Ctrl Pts',(-66.5773555136983,126.999532454046,43.3947223806574));
#24763=CARTESIAN_POINT('Ctrl Pts',(-66.5779451634274,126.999511912239,43.3953057241435));
#24764=CARTESIAN_POINT('Ctrl Pts',(-66.5784244138539,126.999494873465,43.3957799667826));
#24765=CARTESIAN_POINT('Ctrl Pts',(-66.5788673795163,126.999479124722,43.3962183038047));
#24766=CARTESIAN_POINT('Ctrl Pts',(-66.5792155329322,126.999466401456,43.3965629424159));
#24767=CARTESIAN_POINT('Ctrl Pts',(-66.5794881511403,126.999456345864,43.3968329073583));
#24768=CARTESIAN_POINT('Ctrl Pts',(-66.5797414357716,126.999447003396,43.3970837268885));
#24769=CARTESIAN_POINT('Ctrl Pts',(-66.5799293013861,126.999439970325,43.3972698733081));
#24770=CARTESIAN_POINT('Ctrl Pts',(-66.5801001639566,126.999433537031,43.3974392076731));
#24771=CARTESIAN_POINT('Ctrl Pts',(-66.580133469423,126.999432283018,43.3974722152533));
#24772=CARTESIAN_POINT('Ctrl Pts',(-66.5801662412456,126.999431047036,43.3975046952452));
#24773=CARTESIAN_POINT('Ctrl Pts',(-66.5801990080023,126.999429809249,43.3975371703006));
#24774=CARTESIAN_POINT('',(-66.2975371703006,126.999429809249,43.6801990080023));
#24775=CARTESIAN_POINT('Ctrl Pts',(-66.2975371703006,126.999429809249,43.6801990080023));
#24776=CARTESIAN_POINT('Ctrl Pts',(-66.3917577828678,126.999429809249,43.5859783954351));
#24777=CARTESIAN_POINT('Ctrl Pts',(-66.4859783954351,126.999429809249,43.4917577828678));
#24778=CARTESIAN_POINT('Ctrl Pts',(-66.5801990080023,126.999429809249,43.3975371703006));
#24779=CARTESIAN_POINT('',(-66.2677059397486,127.,43.65));
#24780=CARTESIAN_POINT('Ctrl Pts',(-66.2975371703006,126.999429809249,43.6801990080023));
#24781=CARTESIAN_POINT('Ctrl Pts',(-66.2973702471606,126.999436171524,43.6800305855052));
#24782=CARTESIAN_POINT('Ctrl Pts',(-66.2972001071489,126.999442617638,43.6798589093858));
#24783=CARTESIAN_POINT('Ctrl Pts',(-66.296971463311,126.99945117313,43.6796280573389));
#24784=CARTESIAN_POINT('Ctrl Pts',(-66.2967191259022,126.999460615197,43.6793732828919));
#24785=CARTESIAN_POINT('Ctrl Pts',(-66.2963956021262,126.999472627869,43.6790465041628));
#24786=CARTESIAN_POINT('Ctrl Pts',(-66.295973543409,126.999487894907,43.6786200261654));
#24787=CARTESIAN_POINT('Ctrl Pts',(-66.2955021853265,126.999504945239,43.6781437326002));
#24788=CARTESIAN_POINT('Ctrl Pts',(-66.2949084001558,126.999526020176,43.6775435637606));
#24789=CARTESIAN_POINT('Ctrl Pts',(-66.2942060222409,126.999549852402,43.676833440411));
#24790=CARTESIAN_POINT('Ctrl Pts',(-66.2933176689234,126.999579994917,43.6759352908252));
#24791=CARTESIAN_POINT('Ctrl Pts',(-66.2922570121512,126.999614390365,43.6748626694998));
#24792=CARTESIAN_POINT('Ctrl Pts',(-66.2911193310076,126.999648516201,43.6737118227387));
#24793=CARTESIAN_POINT('Ctrl Pts',(-66.2899711196751,126.9996829579,43.6725503239299));
#24794=CARTESIAN_POINT('Ctrl Pts',(-66.288749855389,126.999716919438,43.6713146082227));
#24795=CARTESIAN_POINT('Ctrl Pts',(-66.287554886453,126.999747324912,43.6701051310901));
#24796=CARTESIAN_POINT('Ctrl Pts',(-66.2866600217437,126.999770094362,43.6691994017693));
#24797=CARTESIAN_POINT('Ctrl Pts',(-66.2857804315058,126.999790925398,43.668308923963));
#24798=CARTESIAN_POINT('Ctrl Pts',(-66.284930519969,126.999809700632,43.6674482886095));
#24799=CARTESIAN_POINT('Ctrl Pts',(-66.2841588558683,126.999826747316,43.6666668879845));
#24800=CARTESIAN_POINT('Ctrl Pts',(-66.2834120480745,126.999842123653,43.6659104838894));
#24801=CARTESIAN_POINT('Ctrl Pts',(-66.2826693398963,126.999856381896,43.6651581113809));
#24802=CARTESIAN_POINT('Ctrl Pts',(-66.2818923918,126.999871297464,43.6643710534147));
#24803=CARTESIAN_POINT('Ctrl Pts',(-66.2811127516125,126.999885130105,43.6635811455676));
#24804=CARTESIAN_POINT('Ctrl Pts',(-66.2803056659765,126.999898178282,43.6627634000922));
#24805=CARTESIAN_POINT('Ctrl Pts',(-66.2794046193328,126.999912745528,43.6618504525894));
#24806=CARTESIAN_POINT('Ctrl Pts',(-66.2784699201047,126.999926273619,43.6609033701686));
#24807=CARTESIAN_POINT('Ctrl Pts',(-66.2775198964636,126.999938235568,43.6599407885303));
#24808=CARTESIAN_POINT('Ctrl Pts',(-66.276277873383,126.999953874144,43.6586823476241));
#24809=CARTESIAN_POINT('Ctrl Pts',(-66.2750113535045,126.999966671765,43.6573991342531));
#24810=CARTESIAN_POINT('Ctrl Pts',(-66.2738338670289,126.999975926382,43.6562062234179));
#24811=CARTESIAN_POINT('Ctrl Pts',(-66.2728716751032,126.999983488862,43.6552314273608));
#24812=CARTESIAN_POINT('Ctrl Pts',(-66.2719721616108,126.999988722094,43.6543201973242));
#24813=CARTESIAN_POINT('Ctrl Pts',(-66.2711950841722,126.999992198348,43.6535330697583));
#24814=CARTESIAN_POINT('Ctrl Pts',(-66.2705184152867,126.999995225425,43.6528476493533));
#24815=CARTESIAN_POINT('Ctrl Pts',(-66.2699354824495,126.999996959481,43.6522572394475));
#24816=CARTESIAN_POINT('Ctrl Pts',(-66.2694615957523,126.999998025673,43.6517773349722));
#24817=CARTESIAN_POINT('Ctrl Pts',(-66.2690235842969,126.999999011149,43.6513337613101));
#24818=CARTESIAN_POINT('Ctrl Pts',(-66.2686792256925,126.999999440092,43.6509850931059));
#24819=CARTESIAN_POINT('Ctrl Pts',(-66.2684094978742,126.999999683121,43.6507120440938));
#24820=CARTESIAN_POINT('Ctrl Pts',(-66.268158897172,126.999999908916,43.6504583577125));
#24821=CARTESIAN_POINT('Ctrl Pts',(-66.2679729332258,126.999999972695,43.6502701637938));
#24822=CARTESIAN_POINT('Ctrl Pts',(-66.2678037667737,126.999999993876,43.6500989877776));
#24823=CARTESIAN_POINT('Ctrl Pts',(-66.267770805003,126.999999998003,43.6500656344471));
#24824=CARTESIAN_POINT('Ctrl Pts',(-66.2677383699129,127.,43.6500328147289));
#24825=CARTESIAN_POINT('Ctrl Pts',(-66.2677059397486,127.,43.65));
#24826=CARTESIAN_POINT('',(-66.4088529698743,127.,43.5088529698743));
#24827=CARTESIAN_POINT('Ctrl Pts',(-66.2975371703006,126.999429809249,43.6801990080023));
#24828=CARTESIAN_POINT('Ctrl Pts',(-66.4934491246469,126.991962625601,43.8778707063143));
#24829=CARTESIAN_POINT('Ctrl Pts',(-66.8258588963354,126.852169790253,44.1891309474517));
#24830=CARTESIAN_POINT('Ctrl Pts',(-67.1039178520905,126.497789859875,44.4167876971285));
#24831=CARTESIAN_POINT('Ctrl Pts',(-67.15,126.297687701072,44.45));
#24832=CARTESIAN_POINT('Ctrl Pts',(-67.15,126.2,44.45));
#24833=CARTESIAN_POINT('Ctrl Pts',(-66.3917577828678,126.999429809249,43.5859783954351));
#24834=CARTESIAN_POINT('Ctrl Pts',(-66.5882563185361,126.991962625601,43.7830635124252));
#24835=CARTESIAN_POINT('Ctrl Pts',(-66.9136162467075,126.852169790253,44.1013735970796));
#24836=CARTESIAN_POINT('Ctrl Pts',(-67.1748744671032,126.497789859875,44.3458310821159));
#24837=CARTESIAN_POINT('Ctrl Pts',(-67.2166666666667,126.297687701072,44.3833333333333));
#24838=CARTESIAN_POINT('Ctrl Pts',(-67.2166666666667,126.2,44.3833333333333));
#24839=CARTESIAN_POINT('Ctrl Pts',(-66.4859783954351,126.999429809249,43.4917577828678));
#24840=CARTESIAN_POINT('Ctrl Pts',(-66.6830635124252,126.991962625601,43.6882563185361));
#24841=CARTESIAN_POINT('Ctrl Pts',(-67.0013735970796,126.852169790253,44.0136162467075));
#24842=CARTESIAN_POINT('Ctrl Pts',(-67.2458310821159,126.497789859875,44.2748744671032));
#24843=CARTESIAN_POINT('Ctrl Pts',(-67.2833333333333,126.297687701072,44.3166666666667));
#24844=CARTESIAN_POINT('Ctrl Pts',(-67.2833333333333,126.2,44.3166666666667));
#24845=CARTESIAN_POINT('Ctrl Pts',(-66.5801990080023,126.999429809249,43.3975371703006));
#24846=CARTESIAN_POINT('Ctrl Pts',(-66.7778707063143,126.991962625601,43.5934491246469));
#24847=CARTESIAN_POINT('Ctrl Pts',(-67.0891309474517,126.852169790253,43.9258588963354));
#24848=CARTESIAN_POINT('Ctrl Pts',(-67.3167876971285,126.497789859875,44.2039178520906));
#24849=CARTESIAN_POINT('Ctrl Pts',(-67.35,126.297687701072,44.25));
#24850=CARTESIAN_POINT('Ctrl Pts',(-67.35,126.2,44.25));
#24851=CARTESIAN_POINT('',(-67.35,126.2,44.25));
#24852=CARTESIAN_POINT('Ctrl Pts',(-66.5801990080023,126.999429809249,43.3975371703006));
#24853=CARTESIAN_POINT('Ctrl Pts',(-66.7778707063143,126.991962625601,43.5934491246469));
#24854=CARTESIAN_POINT('Ctrl Pts',(-67.0891309474517,126.852169790253,43.9258588963354));
#24855=CARTESIAN_POINT('Ctrl Pts',(-67.3167876971285,126.497789859875,44.2039178520906));
#24856=CARTESIAN_POINT('Ctrl Pts',(-67.35,126.297687701072,44.25));
#24857=CARTESIAN_POINT('Ctrl Pts',(-67.35,126.2,44.25));
#24858=CARTESIAN_POINT('',(-67.15,126.2,44.45));
#24859=CARTESIAN_POINT('',(-67.35,126.2,44.25));
#24860=CARTESIAN_POINT('Ctrl Pts',(-67.15,126.2,44.45));
#24861=CARTESIAN_POINT('Ctrl Pts',(-67.15,126.297687701072,44.45));
#24862=CARTESIAN_POINT('Ctrl Pts',(-67.1039178520905,126.497789859875,44.4167876971285));
#24863=CARTESIAN_POINT('Ctrl Pts',(-66.8258588963354,126.852169790253,44.1891309474517));
#24864=CARTESIAN_POINT('Ctrl Pts',(-66.4934491246469,126.991962625601,43.8778707063143));
#24865=CARTESIAN_POINT('Ctrl Pts',(-66.2975371703006,126.999429809249,43.6801990080023));
#24866=CARTESIAN_POINT('Origin',(-67.25,122.2375,44.35));
#24867=CARTESIAN_POINT('',(-67.35,123.0375,44.25));
#24868=CARTESIAN_POINT('',(-67.35,122.2375,44.25));
#24869=CARTESIAN_POINT('',(-67.15,123.0375,44.45));
#24870=CARTESIAN_POINT('',(-67.35,123.0375,44.25));
#24871=CARTESIAN_POINT('',(-67.15,122.2375,44.45));
#24872=CARTESIAN_POINT('Ctrl Pts',(-67.15,123.0375,44.45));
#24873=CARTESIAN_POINT('Ctrl Pts',(-67.15,122.964234224196,44.45));
#24874=CARTESIAN_POINT('Ctrl Pts',(-67.124110265378,122.816497863585,44.4310410082707));
#24875=CARTESIAN_POINT('Ctrl Pts',(-66.979153924583,122.559479514224,44.3164595240405));
#24876=CARTESIAN_POINT('Ctrl Pts',(-66.6927364773364,122.319066835802,44.066950725335));
#24877=CARTESIAN_POINT('Ctrl Pts',(-66.4281451398648,122.243048313183,43.8119801402103));
#24878=CARTESIAN_POINT('Ctrl Pts',(-66.2975371703006,122.238070190751,43.6801990080023));
#24879=CARTESIAN_POINT('Ctrl Pts',(-67.2166666666667,123.0375,44.3833333333333));
#24880=CARTESIAN_POINT('Ctrl Pts',(-67.2166666666667,122.964234224196,44.3833333333333));
#24881=CARTESIAN_POINT('Ctrl Pts',(-67.1930871796756,122.816497863585,44.3620640939731));
#24882=CARTESIAN_POINT('Ctrl Pts',(-67.0582557910688,122.559479514224,44.2373576575547));
#24883=CARTESIAN_POINT('Ctrl Pts',(-66.7841412266692,122.319066835802,43.9755459760021));
#24884=CARTESIAN_POINT('Ctrl Pts',(-66.5227568066466,122.243048313183,43.7173684734285));
#24885=CARTESIAN_POINT('Ctrl Pts',(-66.3917577828678,122.238070190751,43.5859783954351));
#24886=CARTESIAN_POINT('Ctrl Pts',(-67.2833333333333,123.0375,44.3166666666667));
#24887=CARTESIAN_POINT('Ctrl Pts',(-67.2833333333333,122.964234224196,44.3166666666667));
#24888=CARTESIAN_POINT('Ctrl Pts',(-67.2620640939731,122.816497863585,44.2930871796756));
#24889=CARTESIAN_POINT('Ctrl Pts',(-67.1373576575547,122.559479514224,44.1582557910688));
#24890=CARTESIAN_POINT('Ctrl Pts',(-66.8755459760021,122.319066835802,43.8841412266693));
#24891=CARTESIAN_POINT('Ctrl Pts',(-66.6173684734285,122.243048313183,43.6227568066467));
#24892=CARTESIAN_POINT('Ctrl Pts',(-66.4859783954351,122.238070190751,43.4917577828678));
#24893=CARTESIAN_POINT('Ctrl Pts',(-67.35,123.0375,44.25));
#24894=CARTESIAN_POINT('Ctrl Pts',(-67.35,122.964234224196,44.25));
#24895=CARTESIAN_POINT('Ctrl Pts',(-67.3310410082707,122.816497863585,44.224110265378));
#24896=CARTESIAN_POINT('Ctrl Pts',(-67.2164595240405,122.559479514224,44.079153924583));
#24897=CARTESIAN_POINT('Ctrl Pts',(-66.966950725335,122.319066835802,43.7927364773364));
#24898=CARTESIAN_POINT('Ctrl Pts',(-66.7119801402103,122.243048313183,43.5281451398648));
#24899=CARTESIAN_POINT('Ctrl Pts',(-66.5801990080023,122.238070190751,43.3975371703006));
#24900=CARTESIAN_POINT('Ctrl Pts',(-66.2975371703006,122.238070190751,43.6801990080023));
#24901=CARTESIAN_POINT('Ctrl Pts',(-66.4281451398648,122.243048313183,43.8119801402103));
#24902=CARTESIAN_POINT('Ctrl Pts',(-66.6927364773364,122.319066835802,44.066950725335));
#24903=CARTESIAN_POINT('Ctrl Pts',(-66.979153924583,122.559479514224,44.3164595240405));
#24904=CARTESIAN_POINT('Ctrl Pts',(-67.124110265378,122.816497863585,44.4310410082707));
#24905=CARTESIAN_POINT('Ctrl Pts',(-67.15,122.964234224196,44.45));
#24906=CARTESIAN_POINT('Ctrl Pts',(-67.15,123.0375,44.45));
#24907=CARTESIAN_POINT('Ctrl Pts',(-67.35,123.0375,44.25));
#24908=CARTESIAN_POINT('Ctrl Pts',(-67.35,122.964234224196,44.25));
#24909=CARTESIAN_POINT('Ctrl Pts',(-67.3310410082707,122.816497863585,44.224110265378));
#24910=CARTESIAN_POINT('Ctrl Pts',(-67.2164595240405,122.559479514224,44.079153924583));
#24911=CARTESIAN_POINT('Ctrl Pts',(-66.966950725335,122.319066835802,43.7927364773364));
#24912=CARTESIAN_POINT('Ctrl Pts',(-66.7119801402103,122.243048313183,43.5281451398648));
#24913=CARTESIAN_POINT('Ctrl Pts',(-66.5801990080023,122.238070190751,43.3975371703006));
#24914=CARTESIAN_POINT('Origin',(-29.25,122.2375,-31.75));
#24915=CARTESIAN_POINT('',(-66.55,122.2375,-106.867705939749));
#24916=CARTESIAN_POINT('',(-66.55,122.2375,-69.85));
#24917=CARTESIAN_POINT('',(-66.2677059397485,122.2375,-107.15));
#24918=CARTESIAN_POINT('',(-66.4088529698743,122.2375,-107.008852969874));
#24919=CARTESIAN_POINT('',(7.76770593974857,122.2375,-107.15));
#24920=CARTESIAN_POINT('',(-10.2,122.2375,-107.15));
#24921=CARTESIAN_POINT('',(8.05,122.2375,-106.867705939749));
#24922=CARTESIAN_POINT('',(7.90885296987428,122.2375,-107.008852969874));
#24923=CARTESIAN_POINT('',(8.05,122.2375,43.3677059397486));
#24924=CARTESIAN_POINT('',(8.05,122.2375,6.35000000000001));
#24925=CARTESIAN_POINT('',(7.76770593974856,122.2375,43.65));
#24926=CARTESIAN_POINT('',(7.90885296987428,122.2375,43.5088529698743));
#24927=CARTESIAN_POINT('',(-48.3,122.2375,43.65));
#24928=CARTESIAN_POINT('Origin',(-66.55,123.0375,-69.85));
#24929=CARTESIAN_POINT('',(-67.35,123.0375,-107.75));
#24930=CARTESIAN_POINT('',(-67.35,123.0375,-69.85));
#24931=CARTESIAN_POINT('',(-66.5801990080023,122.238070190751,-106.897537170301));
#24932=CARTESIAN_POINT('Ctrl Pts',(-66.5801990080023,122.238070190751,-106.897537170301));
#24933=CARTESIAN_POINT('Ctrl Pts',(-66.7778707063143,122.245537374399,-107.093449124647));
#24934=CARTESIAN_POINT('Ctrl Pts',(-67.0891343165395,122.385328730462,-107.425865391595));
#24935=CARTESIAN_POINT('Ctrl Pts',(-67.3167943482721,122.739701425857,-107.703924410673));
#24936=CARTESIAN_POINT('Ctrl Pts',(-67.35,122.939812298928,-107.75));
#24937=CARTESIAN_POINT('Ctrl Pts',(-67.35,123.0375,-107.75));
#24938=CARTESIAN_POINT('Ctrl Pts',(-66.55,122.2375,-106.867705939749));
#24939=CARTESIAN_POINT('Ctrl Pts',(-66.550168736525,122.2375,-106.867872698805));
#24940=CARTESIAN_POINT('Ctrl Pts',(-66.5503407294752,122.237500039141,-106.868042672762));
#24941=CARTESIAN_POINT('Ctrl Pts',(-66.5505719684178,122.237500204467,-106.868271119852));
#24942=CARTESIAN_POINT('Ctrl Pts',(-66.5508271691041,122.237500386926,-106.868523239385));
#24943=CARTESIAN_POINT('Ctrl Pts',(-66.5511544591101,122.23750071898,-106.868846507485));
#24944=CARTESIAN_POINT('Ctrl Pts',(-66.5515815512717,122.237501563317,-106.869268262893));
#24945=CARTESIAN_POINT('Ctrl Pts',(-66.5520585276647,122.237502506272,-106.869739279202));
#24946=CARTESIAN_POINT('Ctrl Pts',(-66.5526595049514,122.237504104656,-106.870332661821));
#24947=CARTESIAN_POINT('Ctrl Pts',(-66.5533705073353,122.237507100231,-106.871034596213));
#24948=CARTESIAN_POINT('Ctrl Pts',(-66.5542697363121,122.237510888837,-106.871922356591));
#24949=CARTESIAN_POINT('Ctrl Pts',(-66.5553435322327,122.237517016609,-106.87298234306));
#24950=CARTESIAN_POINT('Ctrl Pts',(-66.5564954718406,122.237526369906,-106.874119373636));
#24951=CARTESIAN_POINT('Ctrl Pts',(-66.5576581708372,122.237535810566,-106.875267024347));
#24952=CARTESIAN_POINT('Ctrl Pts',(-66.5588950097939,122.237548536479,-106.876487764087));
#24953=CARTESIAN_POINT('Ctrl Pts',(-66.5601053627629,122.237563826519,-106.877682323414));
#24954=CARTESIAN_POINT('Ctrl Pts',(-66.5610117356426,122.237575276466,-106.878576869224));
#24955=CARTESIAN_POINT('Ctrl Pts',(-66.5619027203555,122.237588088159,-106.879456205747));
#24956=CARTESIAN_POINT('Ctrl Pts',(-66.5627636895377,122.237601826337,-106.880305951649));
#24957=CARTESIAN_POINT('Ctrl Pts',(-66.5635453863286,122.237614299594,-106.881077458526));
#24958=CARTESIAN_POINT('Ctrl Pts',(-66.5643019452735,122.237627497267,-106.88182418239));
#24959=CARTESIAN_POINT('Ctrl Pts',(-66.5650543196291,122.237641657879,-106.88256688208));
#24960=CARTESIAN_POINT('Ctrl Pts',(-66.565841390028,122.237656471514,-106.883343831662));
#24961=CARTESIAN_POINT('Ctrl Pts',(-66.5666311424552,122.23767247258,-106.884123555698));
#24962=CARTESIAN_POINT('Ctrl Pts',(-66.567448577761,122.237690305676,-106.884930805518));
#24963=CARTESIAN_POINT('Ctrl Pts',(-66.5683611675107,122.237710214654,-106.885832024129));
#24964=CARTESIAN_POINT('Ctrl Pts',(-66.5693076969374,122.237732447118,-106.886766994225));
#24965=CARTESIAN_POINT('Ctrl Pts',(-66.570269575119,122.237756826022,-106.887717360118));
#24966=CARTESIAN_POINT('Ctrl Pts',(-66.5715270283396,122.237788696306,-106.888959763445));
#24967=CARTESIAN_POINT('Ctrl Pts',(-66.5728089910973,122.237824333784,-106.890226781831));
#24968=CARTESIAN_POINT('Ctrl Pts',(-66.5740006009088,122.237860099072,-106.891404811888));
#24969=CARTESIAN_POINT('Ctrl Pts',(-66.5749744564358,122.237889328626,-106.89236756922));
#24970=CARTESIAN_POINT('Ctrl Pts',(-66.5758847018216,122.237918483815,-106.893267661264));
#24971=CARTESIAN_POINT('Ctrl Pts',(-66.5766709109972,122.237944709537,-106.894045268348));
#24972=CARTESIAN_POINT('Ctrl Pts',(-66.5773555136828,122.237967545954,-106.894722380642));
#24973=CARTESIAN_POINT('Ctrl Pts',(-66.5779451634142,122.23798808776,-106.89530572413));
#24974=CARTESIAN_POINT('Ctrl Pts',(-66.5784244138428,122.238005126534,-106.895779966772));
#24975=CARTESIAN_POINT('Ctrl Pts',(-66.578867379507,122.238020875277,-106.896218303795));
#24976=CARTESIAN_POINT('Ctrl Pts',(-66.5792155329245,122.238033598544,-106.896562942408));
#24977=CARTESIAN_POINT('Ctrl Pts',(-66.5794881511339,122.238043654136,-106.896832907352));
#24978=CARTESIAN_POINT('Ctrl Pts',(-66.5797414357662,122.238052996604,-106.897083726883));
#24979=CARTESIAN_POINT('Ctrl Pts',(-66.5799293013816,122.238060029674,-106.897269873304));
#24980=CARTESIAN_POINT('Ctrl Pts',(-66.5801001639524,122.238066462969,-106.897439207669));
#24981=CARTESIAN_POINT('Ctrl Pts',(-66.5801334694202,122.238067716982,-106.89747221525));
#24982=CARTESIAN_POINT('Ctrl Pts',(-66.5801662412442,122.238068952964,-106.897504695244));
#24983=CARTESIAN_POINT('Ctrl Pts',(-66.5801990080023,122.238070190751,-106.897537170301));
#24984=CARTESIAN_POINT('Origin',(-67.35,122.2375,-107.95));
#24985=CARTESIAN_POINT('',(-67.35,126.2,-107.75));
#24986=CARTESIAN_POINT('',(-67.35,126.2,-69.85));
#24987=CARTESIAN_POINT('',(-67.35,122.2375,-107.75));
#24988=CARTESIAN_POINT('Origin',(-66.55,126.2,-69.85));
#24989=CARTESIAN_POINT('',(-66.55,127.,-106.867705939749));
#24990=CARTESIAN_POINT('',(-66.55,127.,-69.85));
#24991=CARTESIAN_POINT('',(-66.5801990080024,126.999429809249,-106.897537170301));
#24992=CARTESIAN_POINT('Ctrl Pts',(-66.5801990080024,126.999429809249,-106.897537170301));
#24993=CARTESIAN_POINT('Ctrl Pts',(-66.5800305855052,126.999436171524,-106.897370247161));
#24994=CARTESIAN_POINT('Ctrl Pts',(-66.5798589093858,126.999442617638,-106.897200107149));
#24995=CARTESIAN_POINT('Ctrl Pts',(-66.5796280573389,126.99945117313,-106.896971463311));
#24996=CARTESIAN_POINT('Ctrl Pts',(-66.5793732828919,126.999460615197,-106.896719125902));
#24997=CARTESIAN_POINT('Ctrl Pts',(-66.5790465041629,126.999472627869,-106.896395602126));
#24998=CARTESIAN_POINT('Ctrl Pts',(-66.5786200261654,126.999487894907,-106.895973543409));
#24999=CARTESIAN_POINT('Ctrl Pts',(-66.5781437326002,126.999504945239,-106.895502185326));
#25000=CARTESIAN_POINT('Ctrl Pts',(-66.5775435637605,126.999526020176,-106.894908400156));
#25001=CARTESIAN_POINT('Ctrl Pts',(-66.576833440411,126.999549852402,-106.894206022241));
#25002=CARTESIAN_POINT('Ctrl Pts',(-66.5759352908252,126.999579994917,-106.893317668923));
#25003=CARTESIAN_POINT('Ctrl Pts',(-66.5748626694997,126.999614390365,-106.892257012151));
#25004=CARTESIAN_POINT('Ctrl Pts',(-66.5737118227385,126.999648516201,-106.891119331007));
#25005=CARTESIAN_POINT('Ctrl Pts',(-66.5725503239297,126.9996829579,-106.889971119675));
#25006=CARTESIAN_POINT('Ctrl Pts',(-66.5713146082226,126.999716919438,-106.888749855389));
#25007=CARTESIAN_POINT('Ctrl Pts',(-66.5701051310899,126.999747324912,-106.887554886453));
#25008=CARTESIAN_POINT('Ctrl Pts',(-66.5691994017692,126.999770094362,-106.886660021744));
#25009=CARTESIAN_POINT('Ctrl Pts',(-66.5683089239628,126.999790925398,-106.885780431506));
#25010=CARTESIAN_POINT('Ctrl Pts',(-66.5674482886093,126.999809700632,-106.884930519969));
#25011=CARTESIAN_POINT('Ctrl Pts',(-66.5666668879872,126.999826747316,-106.884158855871));
#25012=CARTESIAN_POINT('Ctrl Pts',(-66.5659104838949,126.999842123653,-106.88341204808));
#25013=CARTESIAN_POINT('Ctrl Pts',(-66.5651581113891,126.999856381896,-106.882669339904));
#25014=CARTESIAN_POINT('Ctrl Pts',(-66.5643710534231,126.999871297464,-106.881892391808));
#25015=CARTESIAN_POINT('Ctrl Pts',(-66.5635811455763,126.999885130105,-106.881112751621));
#25016=CARTESIAN_POINT('Ctrl Pts',(-66.5627634001013,126.999898178281,-106.880305665985));
#25017=CARTESIAN_POINT('Ctrl Pts',(-66.5618504525991,126.999912745528,-106.879404619342));
#25018=CARTESIAN_POINT('Ctrl Pts',(-66.5609033701791,126.999926273619,-106.878469920115));
#25019=CARTESIAN_POINT('Ctrl Pts',(-66.5599407885413,126.999938235568,-106.877519896475));
#25020=CARTESIAN_POINT('Ctrl Pts',(-66.5586823476381,126.999953874144,-106.876277873397));
#25021=CARTESIAN_POINT('Ctrl Pts',(-66.55739913427,126.999966671765,-106.875011353521));
#25022=CARTESIAN_POINT('Ctrl Pts',(-66.5562062234366,126.999975926382,-106.873833867047));
#25023=CARTESIAN_POINT('Ctrl Pts',(-66.5552314273775,126.999983488862,-106.87287167512));
#25024=CARTESIAN_POINT('Ctrl Pts',(-66.5543201973387,126.999988722094,-106.871972161625));
#25025=CARTESIAN_POINT('Ctrl Pts',(-66.5535330697706,126.999992198348,-106.871195084184));
#25026=CARTESIAN_POINT('Ctrl Pts',(-66.552847649364,126.999995225425,-106.870518415297));
#25027=CARTESIAN_POINT('Ctrl Pts',(-66.5522572394567,126.999996959481,-106.869935482459));
#25028=CARTESIAN_POINT('Ctrl Pts',(-66.5517773349799,126.999998025673,-106.86946159576));
#25029=CARTESIAN_POINT('Ctrl Pts',(-66.5513337613166,126.999999011149,-106.869023584303));
#25030=CARTESIAN_POINT('Ctrl Pts',(-66.5509850931112,126.999999440092,-106.868679225698));
#25031=CARTESIAN_POINT('Ctrl Pts',(-66.5507120440982,126.999999683121,-106.868409497879));
#25032=CARTESIAN_POINT('Ctrl Pts',(-66.5504583577162,126.999999908916,-106.868158897176));
#25033=CARTESIAN_POINT('Ctrl Pts',(-66.5502701637969,126.999999972695,-106.867972933229));
#25034=CARTESIAN_POINT('Ctrl Pts',(-66.5500989877805,126.999999993876,-106.867803766777));
#25035=CARTESIAN_POINT('Ctrl Pts',(-66.550065634449,126.999999998003,-106.867770805005));
#25036=CARTESIAN_POINT('Ctrl Pts',(-66.5500328147298,127.,-106.867738369914));
#25037=CARTESIAN_POINT('Ctrl Pts',(-66.55,127.,-106.867705939749));
#25038=CARTESIAN_POINT('Ctrl Pts',(-67.35,126.2,-107.75));
#25039=CARTESIAN_POINT('Ctrl Pts',(-67.35,126.297687701072,-107.75));
#25040=CARTESIAN_POINT('Ctrl Pts',(-67.3167946468525,126.497798963876,-107.703924706682));
#25041=CARTESIAN_POINT('Ctrl Pts',(-67.0891344719334,126.852171342114,-107.425865686481));
#25042=CARTESIAN_POINT('Ctrl Pts',(-66.7778707063143,126.991962625601,-107.093449124647));
#25043=CARTESIAN_POINT('Ctrl Pts',(-66.5801990080024,126.999429809249,-106.897537170301));
#25044=CARTESIAN_POINT('Ctrl Pts',(-66.2975371703006,126.999429809249,-107.180199008002));
#25045=CARTESIAN_POINT('Ctrl Pts',(-66.295869694655,126.999493365079,-107.178516554556));
#25046=CARTESIAN_POINT('Ctrl Pts',(-66.2836662133258,126.999932142639,-107.16617353777));
#25047=CARTESIAN_POINT('Ctrl Pts',(-66.270284862015,126.999995925185,-107.152608114732));
#25048=CARTESIAN_POINT('Ctrl Pts',(-66.2681224083043,127.,-107.150421407138));
#25049=CARTESIAN_POINT('Ctrl Pts',(-66.2677059397485,127.,-107.15));
#25050=CARTESIAN_POINT('Ctrl Pts',(-66.3917577828678,126.999429809249,-107.085978395435));
#25051=CARTESIAN_POINT('Ctrl Pts',(-66.390085314622,126.999493365079,-107.084300934589));
#25052=CARTESIAN_POINT('Ctrl Pts',(-66.3778285019322,126.999932142639,-107.072011249164));
#25053=CARTESIAN_POINT('Ctrl Pts',(-66.3643950265928,126.999995925185,-107.058497950154));
#25054=CARTESIAN_POINT('Ctrl Pts',(-66.3622220745824,127.,-107.05632174086));
#25055=CARTESIAN_POINT('Ctrl Pts',(-66.3618039598324,127.,-107.055901979916));
#25056=CARTESIAN_POINT('Ctrl Pts',(-66.4859783954351,126.999429809249,-106.991757782868));
#25057=CARTESIAN_POINT('Ctrl Pts',(-66.484300934589,126.999493365079,-106.990085314622));
#25058=CARTESIAN_POINT('Ctrl Pts',(-66.4719704646475,127.000007510264,-106.977828501932));
#25059=CARTESIAN_POINT('Ctrl Pts',(-66.4584922963115,126.999950446903,-106.964395026593));
#25060=CARTESIAN_POINT('Ctrl Pts',(-66.4563217408604,127.,-106.962222074582));
#25061=CARTESIAN_POINT('Ctrl Pts',(-66.4559019799162,127.,-106.961803959832));
#25062=CARTESIAN_POINT('Ctrl Pts',(-66.5801990080024,126.999429809249,-106.897537170301));
#25063=CARTESIAN_POINT('Ctrl Pts',(-66.578516554556,126.999493365079,-106.895869694655));
#25064=CARTESIAN_POINT('Ctrl Pts',(-66.5661735377701,126.999932142639,-106.883666213326));
#25065=CARTESIAN_POINT('Ctrl Pts',(-66.5526081147318,126.999995925185,-106.870284862015));
#25066=CARTESIAN_POINT('Ctrl Pts',(-66.5504214071384,127.,-106.868122408304));
#25067=CARTESIAN_POINT('Ctrl Pts',(-66.55,127.,-106.867705939749));
#25068=CARTESIAN_POINT('',(-66.2677059397485,127.,-107.15));
#25069=CARTESIAN_POINT('',(-66.2975371703006,126.999429809249,-107.180199008002));
#25070=CARTESIAN_POINT('Ctrl Pts',(-66.2677059397485,127.,-107.15));
#25071=CARTESIAN_POINT('Ctrl Pts',(-66.2678726988052,127.,-107.150168736525));
#25072=CARTESIAN_POINT('Ctrl Pts',(-66.2680426727622,126.999999960859,-107.150340729475));
#25073=CARTESIAN_POINT('Ctrl Pts',(-66.2682711198522,126.999999795533,-107.150571968418));
#25074=CARTESIAN_POINT('Ctrl Pts',(-66.2685232393849,126.999999613074,-107.150827169104));
#25075=CARTESIAN_POINT('Ctrl Pts',(-66.2688465074851,126.99999928102,-107.15115445911));
#25076=CARTESIAN_POINT('Ctrl Pts',(-66.2692682628932,126.999998436683,-107.151581551272));
#25077=CARTESIAN_POINT('Ctrl Pts',(-66.2697392792015,126.999997493728,-107.152058527665));
#25078=CARTESIAN_POINT('Ctrl Pts',(-66.2703326618206,126.999995895344,-107.152659504951));
#25079=CARTESIAN_POINT('Ctrl Pts',(-66.2710345962128,126.999992899769,-107.153370507335));
#25080=CARTESIAN_POINT('Ctrl Pts',(-66.2719223565911,126.999989111163,-107.154269736312));
#25081=CARTESIAN_POINT('Ctrl Pts',(-66.2729823430602,126.999982983391,-107.155343532233));
#25082=CARTESIAN_POINT('Ctrl Pts',(-66.2741193736363,126.999973630094,-107.156495471841));
#25083=CARTESIAN_POINT('Ctrl Pts',(-66.2752670243472,126.999964189434,-107.157658170837));
#25084=CARTESIAN_POINT('Ctrl Pts',(-66.276487764087,126.999951463521,-107.158895009794));
#25085=CARTESIAN_POINT('Ctrl Pts',(-66.2776823234141,126.999936173481,-107.160105362763));
#25086=CARTESIAN_POINT('Ctrl Pts',(-66.2785768692244,126.999924723534,-107.161011735643));
#25087=CARTESIAN_POINT('Ctrl Pts',(-66.2794562057467,126.999911911841,-107.161902720356));
#25088=CARTESIAN_POINT('Ctrl Pts',(-66.280305951649,126.999898173663,-107.162763689538));
#25089=CARTESIAN_POINT('Ctrl Pts',(-66.2810774585299,126.999885700406,-107.163545386333));
#25090=CARTESIAN_POINT('Ctrl Pts',(-66.2818241823979,126.999872502733,-107.164301945281));
#25091=CARTESIAN_POINT('Ctrl Pts',(-66.2825668820916,126.999858342121,-107.165054319641));
#25092=CARTESIAN_POINT('Ctrl Pts',(-66.2833438316739,126.999843528486,-107.16584139004));
#25093=CARTESIAN_POINT('Ctrl Pts',(-66.2841235557099,126.99982752742,-107.166631142468));
#25094=CARTESIAN_POINT('Ctrl Pts',(-66.2849308055304,126.999809694323,-107.167448577774));
#25095=CARTESIAN_POINT('Ctrl Pts',(-66.2858320241426,126.999789785346,-107.168361167525));
#25096=CARTESIAN_POINT('Ctrl Pts',(-66.2867669942401,126.999767552882,-107.169307696952));
#25097=CARTESIAN_POINT('Ctrl Pts',(-66.287717360134,126.999743173978,-107.170269575135));
#25098=CARTESIAN_POINT('Ctrl Pts',(-66.2889597634652,126.999711303693,-107.17152702836));
#25099=CARTESIAN_POINT('Ctrl Pts',(-66.2902267818545,126.999675666215,-107.172808991121));
#25100=CARTESIAN_POINT('Ctrl Pts',(-66.2914048119143,126.999639900927,-107.174000600935));
#25101=CARTESIAN_POINT('Ctrl Pts',(-66.2923675692431,126.999610671373,-107.174974456459));
#25102=CARTESIAN_POINT('Ctrl Pts',(-66.2932676612844,126.999581516184,-107.175884701842));
#25103=CARTESIAN_POINT('Ctrl Pts',(-66.2940452683655,126.999555290462,-107.176670911015));
#25104=CARTESIAN_POINT('Ctrl Pts',(-66.2947223806571,126.999532454046,-107.177355513698));
#25105=CARTESIAN_POINT('Ctrl Pts',(-66.2953057241434,126.999511912239,-107.177945163427));
#25106=CARTESIAN_POINT('Ctrl Pts',(-66.2957799667826,126.999494873465,-107.178424413854));
#25107=CARTESIAN_POINT('Ctrl Pts',(-66.2962183038047,126.999479124722,-107.178867379516));
#25108=CARTESIAN_POINT('Ctrl Pts',(-66.2965629424158,126.999466401456,-107.179215532932));
#25109=CARTESIAN_POINT('Ctrl Pts',(-66.2968329073583,126.999456345864,-107.17948815114));
#25110=CARTESIAN_POINT('Ctrl Pts',(-66.2970837268885,126.999447003396,-107.179741435772));
#25111=CARTESIAN_POINT('Ctrl Pts',(-66.297269873308,126.999439970325,-107.179929301386));
#25112=CARTESIAN_POINT('Ctrl Pts',(-66.297439207673,126.999433537031,-107.180100163957));
#25113=CARTESIAN_POINT('Ctrl Pts',(-66.2974722152532,126.999432283018,-107.180133469423));
#25114=CARTESIAN_POINT('Ctrl Pts',(-66.2975046952452,126.999431047036,-107.180166241246));
#25115=CARTESIAN_POINT('Ctrl Pts',(-66.2975371703006,126.999429809249,-107.180199008002));
#25116=CARTESIAN_POINT('Ctrl Pts',(-66.5801990080024,126.999429809249,-106.897537170301));
#25117=CARTESIAN_POINT('Ctrl Pts',(-66.4859783954351,126.999429809249,-106.991757782868));
#25118=CARTESIAN_POINT('Ctrl Pts',(-66.3917577828678,126.999429809249,-107.085978395435));
#25119=CARTESIAN_POINT('Ctrl Pts',(-66.2975371703006,126.999429809249,-107.180199008002));
#25120=CARTESIAN_POINT('',(-66.4088529698743,127.,-107.008852969874));
#25121=CARTESIAN_POINT('Ctrl Pts',(-66.5801990080023,122.238070190751,-106.897537170301));
#25122=CARTESIAN_POINT('Ctrl Pts',(-66.578516554556,122.238006634921,-106.895869694655));
#25123=CARTESIAN_POINT('Ctrl Pts',(-66.5661734170446,122.237567855022,-106.883666093255));
#25124=CARTESIAN_POINT('Ctrl Pts',(-66.5526080832916,122.237504074413,-106.870284830794));
#25125=CARTESIAN_POINT('Ctrl Pts',(-66.5504214071384,122.2375,-106.868122408304));
#25126=CARTESIAN_POINT('Ctrl Pts',(-66.55,122.2375,-106.867705939749));
#25127=CARTESIAN_POINT('Ctrl Pts',(-66.4859783954351,122.238070190751,-106.991757782868));
#25128=CARTESIAN_POINT('Ctrl Pts',(-66.484300934589,122.238006634921,-106.990085314622));
#25129=CARTESIAN_POINT('Ctrl Pts',(-66.4720111284382,122.237567855022,-106.977828381861));
#25130=CARTESIAN_POINT('Ctrl Pts',(-66.4584979187138,122.237504074413,-106.964394995372));
#25131=CARTESIAN_POINT('Ctrl Pts',(-66.4563217408604,122.2375,-106.962222074582));
#25132=CARTESIAN_POINT('Ctrl Pts',(-66.4559019799162,122.2375,-106.961803959832));
#25133=CARTESIAN_POINT('Ctrl Pts',(-66.3917577828678,122.238070190751,-107.085978395435));
#25134=CARTESIAN_POINT('Ctrl Pts',(-66.390085314622,122.238006634921,-107.084300934589));
#25135=CARTESIAN_POINT('Ctrl Pts',(-66.3778283818612,122.237492501576,-107.07197034337));
#25136=CARTESIAN_POINT('Ctrl Pts',(-66.3643949953721,122.237549556389,-107.058492264776));
#25137=CARTESIAN_POINT('Ctrl Pts',(-66.3622220745824,122.2375,-107.05632174086));
#25138=CARTESIAN_POINT('Ctrl Pts',(-66.3618039598324,122.2375,-107.055901979916));
#25139=CARTESIAN_POINT('Ctrl Pts',(-66.2975371703006,122.238070190751,-107.180199008002));
#25140=CARTESIAN_POINT('Ctrl Pts',(-66.295869694655,122.238006634921,-107.178516554556));
#25141=CARTESIAN_POINT('Ctrl Pts',(-66.2836660932549,122.237567855022,-107.166173417045));
#25142=CARTESIAN_POINT('Ctrl Pts',(-66.2702848307942,122.237504074413,-107.152608083292));
#25143=CARTESIAN_POINT('Ctrl Pts',(-66.2681224083043,122.2375,-107.150421407138));
#25144=CARTESIAN_POINT('Ctrl Pts',(-66.2677059397485,122.2375,-107.15));
#25145=CARTESIAN_POINT('',(-66.2975371703006,122.238070190751,-107.180199008002));
#25146=CARTESIAN_POINT('Ctrl Pts',(-66.2975371703006,122.238070190751,-107.180199008002));
#25147=CARTESIAN_POINT('Ctrl Pts',(-66.3917577828678,122.238070190751,-107.085978395435));
#25148=CARTESIAN_POINT('Ctrl Pts',(-66.4859783954351,122.238070190751,-106.991757782868));
#25149=CARTESIAN_POINT('Ctrl Pts',(-66.5801990080023,122.238070190751,-106.897537170301));
#25150=CARTESIAN_POINT('Ctrl Pts',(-66.2975371703006,122.238070190751,-107.180199008002));
#25151=CARTESIAN_POINT('Ctrl Pts',(-66.2973702471606,122.238063828476,-107.180030585505));
#25152=CARTESIAN_POINT('Ctrl Pts',(-66.2972001071489,122.238057382362,-107.179858909386));
#25153=CARTESIAN_POINT('Ctrl Pts',(-66.296971463311,122.23804882687,-107.179628057339));
#25154=CARTESIAN_POINT('Ctrl Pts',(-66.2967191259022,122.238039384803,-107.179373282892));
#25155=CARTESIAN_POINT('Ctrl Pts',(-66.2963956021262,122.238027372131,-107.179046504163));
#25156=CARTESIAN_POINT('Ctrl Pts',(-66.295973543409,122.238012105093,-107.178620026165));
#25157=CARTESIAN_POINT('Ctrl Pts',(-66.2955021853265,122.237995054761,-107.1781437326));
#25158=CARTESIAN_POINT('Ctrl Pts',(-66.2949084001559,122.237973979824,-107.17754356376));
#25159=CARTESIAN_POINT('Ctrl Pts',(-66.2942060222409,122.237950147598,-107.176833440411));
#25160=CARTESIAN_POINT('Ctrl Pts',(-66.2933176689234,122.237920005083,-107.175935290825));
#25161=CARTESIAN_POINT('Ctrl Pts',(-66.2922570121511,122.237885609635,-107.1748626695));
#25162=CARTESIAN_POINT('Ctrl Pts',(-66.2911193310074,122.237851483799,-107.173711822738));
#25163=CARTESIAN_POINT('Ctrl Pts',(-66.289971119675,122.2378170421,-107.17255032393));
#25164=CARTESIAN_POINT('Ctrl Pts',(-66.2887498553889,122.237783080562,-107.171314608223));
#25165=CARTESIAN_POINT('Ctrl Pts',(-66.2875548864529,122.237752675088,-107.17010513109));
#25166=CARTESIAN_POINT('Ctrl Pts',(-66.2866600217435,122.237729905638,-107.169199401769));
#25167=CARTESIAN_POINT('Ctrl Pts',(-66.2857804315056,122.237709074602,-107.168308923963));
#25168=CARTESIAN_POINT('Ctrl Pts',(-66.2849305199686,122.237690299368,-107.167448288609));
#25169=CARTESIAN_POINT('Ctrl Pts',(-66.2841588558709,122.237673252684,-107.166666887987));
#25170=CARTESIAN_POINT('Ctrl Pts',(-66.2834120480798,122.237657876347,-107.165910483895));
#25171=CARTESIAN_POINT('Ctrl Pts',(-66.2826693399044,122.237643618104,-107.165158111389));
#25172=CARTESIAN_POINT('Ctrl Pts',(-66.2818923918083,122.237628702536,-107.164371053423));
#25173=CARTESIAN_POINT('Ctrl Pts',(-66.2811127516211,122.237614869895,-107.163581145576));
#25174=CARTESIAN_POINT('Ctrl Pts',(-66.2803056659855,122.237601821719,-107.162763400101));
#25175=CARTESIAN_POINT('Ctrl Pts',(-66.2794046193424,122.237587254472,-107.161850452599));
#25176=CARTESIAN_POINT('Ctrl Pts',(-66.2784699201151,122.237573726381,-107.160903370179));
#25177=CARTESIAN_POINT('Ctrl Pts',(-66.2775198964746,122.237561764432,-107.159940788541));
#25178=CARTESIAN_POINT('Ctrl Pts',(-66.276277873397,122.237546125856,-107.158682347638));
#25179=CARTESIAN_POINT('Ctrl Pts',(-66.2750113535215,122.237533328235,-107.15739913427));
#25180=CARTESIAN_POINT('Ctrl Pts',(-66.2738338670477,122.237524073618,-107.156206223437));
#25181=CARTESIAN_POINT('Ctrl Pts',(-66.27287167512,122.237516511138,-107.155231427378));
#25182=CARTESIAN_POINT('Ctrl Pts',(-66.2719721616253,122.237511277906,-107.154320197339));
#25183=CARTESIAN_POINT('Ctrl Pts',(-66.2711950841845,122.237507801652,-107.153533069771));
#25184=CARTESIAN_POINT('Ctrl Pts',(-66.2705184152976,122.237504774575,-107.152847649364));
#25185=CARTESIAN_POINT('Ctrl Pts',(-66.2699354824588,122.237503040519,-107.152257239457));
#25186=CARTESIAN_POINT('Ctrl Pts',(-66.2694615957603,122.237501974327,-107.15177733498));
#25187=CARTESIAN_POINT('Ctrl Pts',(-66.2690235843036,122.237500988851,-107.151333761317));
#25188=CARTESIAN_POINT('Ctrl Pts',(-66.2686792256979,122.237500559908,-107.150985093111));
#25189=CARTESIAN_POINT('Ctrl Pts',(-66.2684094978787,122.237500316879,-107.150712044098));
#25190=CARTESIAN_POINT('Ctrl Pts',(-66.2681588971757,122.237500091084,-107.150458357716));
#25191=CARTESIAN_POINT('Ctrl Pts',(-66.2679729332289,122.237500027304,-107.150270163797));
#25192=CARTESIAN_POINT('Ctrl Pts',(-66.2678037667766,122.237500006124,-107.150098987781));
#25193=CARTESIAN_POINT('Ctrl Pts',(-66.2677708050049,122.237500001997,-107.150065634449));
#25194=CARTESIAN_POINT('Ctrl Pts',(-66.2677383699138,122.2375,-107.15003281473));
#25195=CARTESIAN_POINT('Ctrl Pts',(-66.2677059397485,122.2375,-107.15));
#25196=CARTESIAN_POINT('Ctrl Pts',(-66.2975371703006,122.238070190751,-107.180199008002));
#25197=CARTESIAN_POINT('Ctrl Pts',(-66.4934491246469,122.245537374399,-107.377870706314));
#25198=CARTESIAN_POINT('Ctrl Pts',(-66.8258653915954,122.385328730462,-107.689134316539));
#25199=CARTESIAN_POINT('Ctrl Pts',(-67.1039244106735,122.739701425857,-107.916794348272));
#25200=CARTESIAN_POINT('Ctrl Pts',(-67.15,122.939812298928,-107.95));
#25201=CARTESIAN_POINT('Ctrl Pts',(-67.15,123.0375,-107.95));
#25202=CARTESIAN_POINT('Ctrl Pts',(-66.3917577828678,122.238070190751,-107.085978395435));
#25203=CARTESIAN_POINT('Ctrl Pts',(-66.5882563185361,122.245537374399,-107.283063512425));
#25204=CARTESIAN_POINT('Ctrl Pts',(-66.9136216999101,122.385328730462,-107.601378008225));
#25205=CARTESIAN_POINT('Ctrl Pts',(-67.1748810565397,122.739701425857,-107.845837702406));
#25206=CARTESIAN_POINT('Ctrl Pts',(-67.2166666666667,122.939812298928,-107.883333333333));
#25207=CARTESIAN_POINT('Ctrl Pts',(-67.2166666666667,123.0375,-107.883333333333));
#25208=CARTESIAN_POINT('Ctrl Pts',(-66.4859783954351,122.238070190751,-106.991757782868));
#25209=CARTESIAN_POINT('Ctrl Pts',(-66.6830635124252,122.245537374399,-107.188256318536));
#25210=CARTESIAN_POINT('Ctrl Pts',(-67.0013780082248,122.385328730462,-107.51362169991));
#25211=CARTESIAN_POINT('Ctrl Pts',(-67.2458377024059,122.739701425857,-107.77488105654));
#25212=CARTESIAN_POINT('Ctrl Pts',(-67.2833333333333,122.939812298928,-107.816666666667));
#25213=CARTESIAN_POINT('Ctrl Pts',(-67.2833333333333,123.0375,-107.816666666667));
#25214=CARTESIAN_POINT('Ctrl Pts',(-66.5801990080023,122.238070190751,-106.897537170301));
#25215=CARTESIAN_POINT('Ctrl Pts',(-66.7778707063143,122.245537374399,-107.093449124647));
#25216=CARTESIAN_POINT('Ctrl Pts',(-67.0891343165395,122.385328730462,-107.425865391595));
#25217=CARTESIAN_POINT('Ctrl Pts',(-67.3167943482721,122.739701425857,-107.703924410673));
#25218=CARTESIAN_POINT('Ctrl Pts',(-67.35,122.939812298928,-107.75));
#25219=CARTESIAN_POINT('Ctrl Pts',(-67.35,123.0375,-107.75));
#25220=CARTESIAN_POINT('',(-67.15,123.0375,-107.95));
#25221=CARTESIAN_POINT('',(-67.35,123.0375,-107.75));
#25222=CARTESIAN_POINT('Ctrl Pts',(-67.15,123.0375,-107.95));
#25223=CARTESIAN_POINT('Ctrl Pts',(-67.15,122.939812298928,-107.95));
#25224=CARTESIAN_POINT('Ctrl Pts',(-67.1039244106735,122.739701425857,-107.916794348272));
#25225=CARTESIAN_POINT('Ctrl Pts',(-66.8258653915954,122.385328730462,-107.689134316539));
#25226=CARTESIAN_POINT('Ctrl Pts',(-66.4934491246469,122.245537374399,-107.377870706314));
#25227=CARTESIAN_POINT('Ctrl Pts',(-66.2975371703006,122.238070190751,-107.180199008002));
#25228=CARTESIAN_POINT('Origin',(-67.25,122.2375,-107.85));
#25229=CARTESIAN_POINT('',(-67.15,126.2,-107.95));
#25230=CARTESIAN_POINT('',(-67.35,126.2,-107.75));
#25231=CARTESIAN_POINT('',(-67.15,122.2375,-107.95));
#25232=CARTESIAN_POINT('Ctrl Pts',(-66.5801990080024,126.999429809249,-106.897537170301));
#25233=CARTESIAN_POINT('Ctrl Pts',(-66.7778707063143,126.991962625601,-107.093449124647));
#25234=CARTESIAN_POINT('Ctrl Pts',(-67.0891344719334,126.852171342114,-107.425865686481));
#25235=CARTESIAN_POINT('Ctrl Pts',(-67.3167946468525,126.497798963876,-107.703924706682));
#25236=CARTESIAN_POINT('Ctrl Pts',(-67.35,126.297687701072,-107.75));
#25237=CARTESIAN_POINT('Ctrl Pts',(-67.35,126.2,-107.75));
#25238=CARTESIAN_POINT('Ctrl Pts',(-66.4859783954351,126.999429809249,-106.991757782868));
#25239=CARTESIAN_POINT('Ctrl Pts',(-66.6830635124252,126.991962625601,-107.188256318536));
#25240=CARTESIAN_POINT('Ctrl Pts',(-67.0013782101158,126.852171342114,-107.513621948298));
#25241=CARTESIAN_POINT('Ctrl Pts',(-67.2458380001291,126.497798963876,-107.774881353406));
#25242=CARTESIAN_POINT('Ctrl Pts',(-67.2833333333333,126.297687701072,-107.816666666667));
#25243=CARTESIAN_POINT('Ctrl Pts',(-67.2833333333333,126.2,-107.816666666667));
#25244=CARTESIAN_POINT('Ctrl Pts',(-66.3917577828678,126.999429809249,-107.085978395435));
#25245=CARTESIAN_POINT('Ctrl Pts',(-66.5882563185361,126.991962625601,-107.283063512425));
#25246=CARTESIAN_POINT('Ctrl Pts',(-66.9136219482982,126.852171342114,-107.601378210116));
#25247=CARTESIAN_POINT('Ctrl Pts',(-67.1748813534057,126.497798963876,-107.845838000129));
#25248=CARTESIAN_POINT('Ctrl Pts',(-67.2166666666667,126.297687701072,-107.883333333333));
#25249=CARTESIAN_POINT('Ctrl Pts',(-67.2166666666667,126.2,-107.883333333333));
#25250=CARTESIAN_POINT('Ctrl Pts',(-66.2975371703006,126.999429809249,-107.180199008002));
#25251=CARTESIAN_POINT('Ctrl Pts',(-66.4934491246469,126.991962625601,-107.377870706314));
#25252=CARTESIAN_POINT('Ctrl Pts',(-66.8258656864805,126.852171342114,-107.689134471933));
#25253=CARTESIAN_POINT('Ctrl Pts',(-67.1039247066823,126.497798963876,-107.916794646852));
#25254=CARTESIAN_POINT('Ctrl Pts',(-67.15,126.297687701072,-107.95));
#25255=CARTESIAN_POINT('Ctrl Pts',(-67.15,126.2,-107.95));
#25256=CARTESIAN_POINT('Ctrl Pts',(-66.2975371703006,126.999429809249,-107.180199008002));
#25257=CARTESIAN_POINT('Ctrl Pts',(-66.4934491246469,126.991962625601,-107.377870706314));
#25258=CARTESIAN_POINT('Ctrl Pts',(-66.8258656864805,126.852171342114,-107.689134471933));
#25259=CARTESIAN_POINT('Ctrl Pts',(-67.1039247066823,126.497798963876,-107.916794646852));
#25260=CARTESIAN_POINT('Ctrl Pts',(-67.15,126.297687701072,-107.95));
#25261=CARTESIAN_POINT('Ctrl Pts',(-67.15,126.2,-107.95));
#25262=CARTESIAN_POINT('Ctrl Pts',(7.79753717030057,122.238070190751,-107.180199008002));
#25263=CARTESIAN_POINT('Ctrl Pts',(7.79586969465498,122.238006634921,-107.178516554556));
#25264=CARTESIAN_POINT('Ctrl Pts',(7.78366424106801,122.237567818931,-107.166171554764));
#25265=CARTESIAN_POINT('Ctrl Pts',(7.77028435014845,122.23750406825,-107.152607599263));
#25266=CARTESIAN_POINT('Ctrl Pts',(7.76812240830435,122.2375,-107.150421407138));
#25267=CARTESIAN_POINT('Ctrl Pts',(7.76770593974856,122.2375,-107.15));
#25268=CARTESIAN_POINT('Ctrl Pts',(7.89175778286783,122.238070190751,-107.085978395435));
#25269=CARTESIAN_POINT('Ctrl Pts',(7.890085314622,122.238006634921,-107.084300934589));
#25270=CARTESIAN_POINT('Ctrl Pts',(7.87782652967437,122.237567818931,-107.072009266158));
#25271=CARTESIAN_POINT('Ctrl Pts',(7.8643945147263,122.23750406825,-107.058497434685));
#25272=CARTESIAN_POINT('Ctrl Pts',(7.86222207458238,122.2375,-107.05632174086));
#25273=CARTESIAN_POINT('Ctrl Pts',(7.86180395983237,122.2375,-107.055901979916));
#25274=CARTESIAN_POINT('Ctrl Pts',(7.98597839543508,122.238070190751,-106.991757782868));
#25275=CARTESIAN_POINT('Ctrl Pts',(7.98430093458903,122.238006634921,-106.990085314622));
#25276=CARTESIAN_POINT('Ctrl Pts',(7.97196847256973,122.237492684192,-106.977826529674));
#25277=CARTESIAN_POINT('Ctrl Pts',(7.95849177929169,122.237549607091,-106.964394514726));
#25278=CARTESIAN_POINT('Ctrl Pts',(7.9563217408604,122.2375,-106.962222074582));
#25279=CARTESIAN_POINT('Ctrl Pts',(7.95590197991618,122.2375,-106.961803959832));
#25280=CARTESIAN_POINT('Ctrl Pts',(8.08019900800234,122.238070190751,-106.897537170301));
#25281=CARTESIAN_POINT('Ctrl Pts',(8.07851655455605,122.238006634921,-106.895869694655));
#25282=CARTESIAN_POINT('Ctrl Pts',(8.06617155476444,122.237567818931,-106.883664241068));
#25283=CARTESIAN_POINT('Ctrl Pts',(8.05260759926268,122.23750406825,-106.870284350148));
#25284=CARTESIAN_POINT('Ctrl Pts',(8.05042140713842,122.2375,-106.868122408304));
#25285=CARTESIAN_POINT('Ctrl Pts',(8.04999999999999,122.2375,-106.867705939749));
#25286=CARTESIAN_POINT('',(7.79753717030057,122.238070190751,-107.180199008002));
#25287=CARTESIAN_POINT('Ctrl Pts',(7.76770593974857,122.2375,-107.15));
#25288=CARTESIAN_POINT('Ctrl Pts',(7.76787269880524,122.2375,-107.150168736525));
#25289=CARTESIAN_POINT('Ctrl Pts',(7.76804267276228,122.237500039141,-107.150340729475));
#25290=CARTESIAN_POINT('Ctrl Pts',(7.76827111985225,122.237500204467,-107.150571968418));
#25291=CARTESIAN_POINT('Ctrl Pts',(7.76852323938491,122.237500386926,-107.150827169104));
#25292=CARTESIAN_POINT('Ctrl Pts',(7.76884650748517,122.23750071898,-107.15115445911));
#25293=CARTESIAN_POINT('Ctrl Pts',(7.76926826289328,122.237501563317,-107.151581551272));
#25294=CARTESIAN_POINT('Ctrl Pts',(7.76973927920157,122.237502506272,-107.152058527665));
#25295=CARTESIAN_POINT('Ctrl Pts',(7.77033266182064,122.237504104656,-107.152659504951));
#25296=CARTESIAN_POINT('Ctrl Pts',(7.77103459621282,122.237507100231,-107.153370507335));
#25297=CARTESIAN_POINT('Ctrl Pts',(7.77192235659105,122.237510888837,-107.154269736312));
#25298=CARTESIAN_POINT('Ctrl Pts',(7.77298234306013,122.237517016609,-107.155343532233));
#25299=CARTESIAN_POINT('Ctrl Pts',(7.7741193736361,122.237526369906,-107.15649547184));
#25300=CARTESIAN_POINT('Ctrl Pts',(7.77526702434705,122.237535810566,-107.157658170837));
#25301=CARTESIAN_POINT('Ctrl Pts',(7.77648776408678,122.237548536479,-107.158895009794));
#25302=CARTESIAN_POINT('Ctrl Pts',(7.77768232341393,122.237563826519,-107.160105362763));
#25303=CARTESIAN_POINT('Ctrl Pts',(7.77857686922413,122.237575276466,-107.161011735642));
#25304=CARTESIAN_POINT('Ctrl Pts',(7.77945620574639,122.237588088159,-107.161902720355));
#25305=CARTESIAN_POINT('Ctrl Pts',(7.78030595164864,122.237601826337,-107.162763689537));
#25306=CARTESIAN_POINT('Ctrl Pts',(7.78107745853227,122.237614299594,-107.163545386335));
#25307=CARTESIAN_POINT('Ctrl Pts',(7.78182418240277,122.237627497267,-107.164301945286));
#25308=CARTESIAN_POINT('Ctrl Pts',(7.78256688209903,122.237641657879,-107.165054319648));
#25309=CARTESIAN_POINT('Ctrl Pts',(7.78334383168152,122.237656471514,-107.165841390048));
#25310=CARTESIAN_POINT('Ctrl Pts',(7.78412355571779,122.23767247258,-107.166631142476));
#25311=CARTESIAN_POINT('Ctrl Pts',(7.78493080553857,122.237690305677,-107.167448577782));
#25312=CARTESIAN_POINT('Ctrl Pts',(7.78583202415144,122.237710214654,-107.168361167533));
#25313=CARTESIAN_POINT('Ctrl Pts',(7.78676699424957,122.237732447119,-107.169307696962));
#25314=CARTESIAN_POINT('Ctrl Pts',(7.78771736014403,122.237756826023,-107.170269575145));
#25315=CARTESIAN_POINT('Ctrl Pts',(7.78895976347825,122.237788696307,-107.171527028373));
#25316=CARTESIAN_POINT('Ctrl Pts',(7.79022678187039,122.237824333785,-107.172808991137));
#25317=CARTESIAN_POINT('Ctrl Pts',(7.79140481193201,122.237860099073,-107.174000600953));
#25318=CARTESIAN_POINT('Ctrl Pts',(7.79236756925898,122.237889328628,-107.174974456476));
#25319=CARTESIAN_POINT('Ctrl Pts',(7.79326766129812,122.237918483816,-107.175884701856));
#25320=CARTESIAN_POINT('Ctrl Pts',(7.79404526837716,122.237944709538,-107.176670911026));
#25321=CARTESIAN_POINT('Ctrl Pts',(7.79472238066739,122.237967545954,-107.177355513708));
#25322=CARTESIAN_POINT('Ctrl Pts',(7.79530572415215,122.237988087761,-107.177945163436));
#25323=CARTESIAN_POINT('Ctrl Pts',(7.79577996678998,122.238005126535,-107.178424413861));
#25324=CARTESIAN_POINT('Ctrl Pts',(7.79621830381088,122.238020875278,-107.178867379523));
#25325=CARTESIAN_POINT('Ctrl Pts',(7.79656294242096,122.238033598544,-107.179215532937));
#25326=CARTESIAN_POINT('Ctrl Pts',(7.79683290736253,122.238043654136,-107.179488151145));
#25327=CARTESIAN_POINT('Ctrl Pts',(7.79708372689204,122.238052996604,-107.179741435775));
#25328=CARTESIAN_POINT('Ctrl Pts',(7.79726987331101,122.238060029675,-107.179929301389));
#25329=CARTESIAN_POINT('Ctrl Pts',(7.79743920767582,122.238066462969,-107.180100163959));
#25330=CARTESIAN_POINT('Ctrl Pts',(7.79747221525505,122.238067716982,-107.180133469425));
#25331=CARTESIAN_POINT('Ctrl Pts',(7.79750469524612,122.238068952964,-107.180166241246));
#25332=CARTESIAN_POINT('Ctrl Pts',(7.79753717030058,122.238070190751,-107.180199008002));
#25333=CARTESIAN_POINT('',(8.08019900800234,122.238070190751,-106.897537170301));
#25334=CARTESIAN_POINT('Ctrl Pts',(8.08019900800234,122.238070190751,-106.897537170301));
#25335=CARTESIAN_POINT('Ctrl Pts',(7.98597839543508,122.238070190751,-106.991757782868));
#25336=CARTESIAN_POINT('Ctrl Pts',(7.89175778286783,122.238070190751,-107.085978395435));
#25337=CARTESIAN_POINT('Ctrl Pts',(7.79753717030057,122.238070190751,-107.180199008002));
#25338=CARTESIAN_POINT('Ctrl Pts',(8.08019900800234,122.238070190751,-106.897537170301));
#25339=CARTESIAN_POINT('Ctrl Pts',(8.08003058550519,122.238063828476,-106.897370247161));
#25340=CARTESIAN_POINT('Ctrl Pts',(8.07985890938578,122.238057382362,-106.897200107149));
#25341=CARTESIAN_POINT('Ctrl Pts',(8.07962805733886,122.23804882687,-106.896971463311));
#25342=CARTESIAN_POINT('Ctrl Pts',(8.07937328289186,122.238039384803,-106.896719125902));
#25343=CARTESIAN_POINT('Ctrl Pts',(8.0790465041628,122.238027372131,-106.896395602126));
#25344=CARTESIAN_POINT('Ctrl Pts',(8.07862002616534,122.238012105093,-106.895973543409));
#25345=CARTESIAN_POINT('Ctrl Pts',(8.07814373260017,122.237995054761,-106.895502185326));
#25346=CARTESIAN_POINT('Ctrl Pts',(8.07754356376052,122.237973979824,-106.894908400156));
#25347=CARTESIAN_POINT('Ctrl Pts',(8.07683344041101,122.237950147598,-106.894206022241));
#25348=CARTESIAN_POINT('Ctrl Pts',(8.07593529082528,122.237920005083,-106.893317668923));
#25349=CARTESIAN_POINT('Ctrl Pts',(8.07486266949997,122.237885609635,-106.892257012151));
#25350=CARTESIAN_POINT('Ctrl Pts',(8.07371182273889,122.237851483799,-106.891119331008));
#25351=CARTESIAN_POINT('Ctrl Pts',(8.07255032393007,122.2378170421,-106.889971119675));
#25352=CARTESIAN_POINT('Ctrl Pts',(8.07131460822295,122.237783080562,-106.888749855389));
#25353=CARTESIAN_POINT('Ctrl Pts',(8.07010513109027,122.237752675088,-106.887554886453));
#25354=CARTESIAN_POINT('Ctrl Pts',(8.06919940176948,122.237729905638,-106.886660021744));
#25355=CARTESIAN_POINT('Ctrl Pts',(8.06830892396311,122.237709074602,-106.885780431506));
#25356=CARTESIAN_POINT('Ctrl Pts',(8.06744828860957,122.237690299368,-106.884930519969));
#25357=CARTESIAN_POINT('Ctrl Pts',(8.06666688798671,122.237673252684,-106.88415885587));
#25358=CARTESIAN_POINT('Ctrl Pts',(8.06591048389357,122.237657876347,-106.883412048079));
#25359=CARTESIAN_POINT('Ctrl Pts',(8.06515811138706,122.237643618104,-106.882669339902));
#25360=CARTESIAN_POINT('Ctrl Pts',(8.06437105342106,122.237628702536,-106.881892391806));
#25361=CARTESIAN_POINT('Ctrl Pts',(8.06358114557415,122.237614869895,-106.881112751619));
#25362=CARTESIAN_POINT('Ctrl Pts',(8.06276340009909,122.237601821719,-106.880305665983));
#25363=CARTESIAN_POINT('Ctrl Pts',(8.06185045259669,122.237587254472,-106.87940461934));
#25364=CARTESIAN_POINT('Ctrl Pts',(8.06090337017639,122.237573726381,-106.878469920113));
#25365=CARTESIAN_POINT('Ctrl Pts',(8.05994078853847,122.237561764432,-106.877519896472));
#25366=CARTESIAN_POINT('Ctrl Pts',(8.05868234763433,122.237546125856,-106.876277873393));
#25367=CARTESIAN_POINT('Ctrl Pts',(8.0573991342653,122.237533328235,-106.875011353517));
#25368=CARTESIAN_POINT('Ctrl Pts',(8.05620622343127,122.237524073618,-106.873833867042));
#25369=CARTESIAN_POINT('Ctrl Pts',(8.05523142737274,122.237516511138,-106.872871675115));
#25370=CARTESIAN_POINT('Ctrl Pts',(8.05432019733458,122.237511277906,-106.871972161621));
#25371=CARTESIAN_POINT('Ctrl Pts',(8.0535330697671,122.237507801652,-106.871195084181));
#25372=CARTESIAN_POINT('Ctrl Pts',(8.05284764936096,122.237504774575,-106.870518415294));
#25373=CARTESIAN_POINT('Ctrl Pts',(8.0522572394541,122.237503040519,-106.869935482456));
#25374=CARTESIAN_POINT('Ctrl Pts',(8.05177733497778,122.237501974327,-106.869461595758));
#25375=CARTESIAN_POINT('Ctrl Pts',(8.0513337613147,122.237500988851,-106.869023584302));
#25376=CARTESIAN_POINT('Ctrl Pts',(8.05098509310967,122.237500559908,-106.868679225696));
#25377=CARTESIAN_POINT('Ctrl Pts',(8.05071204409691,122.237500316879,-106.868409497877));
#25378=CARTESIAN_POINT('Ctrl Pts',(8.0504583577151,122.237500091084,-106.868158897175));
#25379=CARTESIAN_POINT('Ctrl Pts',(8.05027016379602,122.237500027304,-106.867972933228));
#25380=CARTESIAN_POINT('Ctrl Pts',(8.0500989877797,122.237500006124,-106.867803766776));
#25381=CARTESIAN_POINT('Ctrl Pts',(8.05006563444842,122.237500001997,-106.867770805004));
#25382=CARTESIAN_POINT('Ctrl Pts',(8.05003281472958,122.2375,-106.867738369914));
#25383=CARTESIAN_POINT('Ctrl Pts',(8.05,122.2375,-106.867705939749));
#25384=CARTESIAN_POINT('Ctrl Pts',(8.08019900800235,126.999429809249,-106.897537170301));
#25385=CARTESIAN_POINT('Ctrl Pts',(8.07851655455606,126.999493365079,-106.895869694655));
#25386=CARTESIAN_POINT('Ctrl Pts',(8.06617173861538,126.999932177505,-106.883664423923));
#25387=CARTESIAN_POINT('Ctrl Pts',(8.05260764696713,126.999995931145,-106.870284397519));
#25388=CARTESIAN_POINT('Ctrl Pts',(8.05042140713843,127.,-106.868122408304));
#25389=CARTESIAN_POINT('Ctrl Pts',(8.05,127.,-106.867705939749));
#25390=CARTESIAN_POINT('Ctrl Pts',(7.9859783954351,126.999429809249,-106.991757782868));
#25391=CARTESIAN_POINT('Ctrl Pts',(7.98430093458904,126.999493365079,-106.990085314622));
#25392=CARTESIAN_POINT('Ctrl Pts',(7.97200945000902,126.999932177505,-106.977826712529));
#25393=CARTESIAN_POINT('Ctrl Pts',(7.95849748238928,126.999995931145,-106.964394562097));
#25394=CARTESIAN_POINT('Ctrl Pts',(7.95632174086041,127.,-106.962222074582));
#25395=CARTESIAN_POINT('Ctrl Pts',(7.95590197991619,127.,-106.961803959832));
#25396=CARTESIAN_POINT('Ctrl Pts',(7.89175778286785,126.999429809249,-107.085978395435));
#25397=CARTESIAN_POINT('Ctrl Pts',(7.89008531462202,126.999493365079,-107.084300934589));
#25398=CARTESIAN_POINT('Ctrl Pts',(7.8778267125293,127.000007333835,-107.071968657262));
#25399=CARTESIAN_POINT('Ctrl Pts',(7.86439456209684,126.999950397908,-107.058491827139));
#25400=CARTESIAN_POINT('Ctrl Pts',(7.86222207458239,127.,-107.05632174086));
#25401=CARTESIAN_POINT('Ctrl Pts',(7.86180395983238,127.,-107.055901979916));
#25402=CARTESIAN_POINT('Ctrl Pts',(7.7975371703006,126.999429809249,-107.180199008002));
#25403=CARTESIAN_POINT('Ctrl Pts',(7.795869694655,126.999493365079,-107.178516554556));
#25404=CARTESIAN_POINT('Ctrl Pts',(7.78366442392293,126.999932177505,-107.166171738615));
#25405=CARTESIAN_POINT('Ctrl Pts',(7.77028439751899,126.999995931145,-107.152607646967));
#25406=CARTESIAN_POINT('Ctrl Pts',(7.76812240830436,127.,-107.150421407138));
#25407=CARTESIAN_POINT('Ctrl Pts',(7.76770593974857,127.,-107.15));
#25408=CARTESIAN_POINT('',(8.05,127.,-106.867705939749));
#25409=CARTESIAN_POINT('',(8.08019900800235,126.999429809249,-106.897537170301));
#25410=CARTESIAN_POINT('Ctrl Pts',(8.05,127.,-106.867705939749));
#25411=CARTESIAN_POINT('Ctrl Pts',(8.05016873652501,127.,-106.867872698805));
#25412=CARTESIAN_POINT('Ctrl Pts',(8.05034072947524,126.999999960859,-106.868042672762));
#25413=CARTESIAN_POINT('Ctrl Pts',(8.05057196841784,126.999999795533,-106.868271119852));
#25414=CARTESIAN_POINT('Ctrl Pts',(8.05082716910411,126.999999613074,-106.868523239385));
#25415=CARTESIAN_POINT('Ctrl Pts',(8.05115445911008,126.99999928102,-106.868846507485));
#25416=CARTESIAN_POINT('Ctrl Pts',(8.0515815512717,126.999998436683,-106.869268262893));
#25417=CARTESIAN_POINT('Ctrl Pts',(8.05205852766472,126.999997493728,-106.869739279202));
#25418=CARTESIAN_POINT('Ctrl Pts',(8.05265950495146,126.999995895344,-106.870332661821));
#25419=CARTESIAN_POINT('Ctrl Pts',(8.05337050733543,126.999992899769,-106.871034596213));
#25420=CARTESIAN_POINT('Ctrl Pts',(8.05426973631222,126.999989111163,-106.871922356591));
#25421=CARTESIAN_POINT('Ctrl Pts',(8.05534353223281,126.999982983391,-106.87298234306));
#25422=CARTESIAN_POINT('Ctrl Pts',(8.05649547184056,126.999973630094,-106.874119373636));
#25423=CARTESIAN_POINT('Ctrl Pts',(8.05765817083721,126.999964189434,-106.875267024347));
#25424=CARTESIAN_POINT('Ctrl Pts',(8.05889500979385,126.999951463521,-106.876487764087));
#25425=CARTESIAN_POINT('Ctrl Pts',(8.06010536276288,126.999936173481,-106.877682323414));
#25426=CARTESIAN_POINT('Ctrl Pts',(8.06101173564262,126.999924723534,-106.878576869224));
#25427=CARTESIAN_POINT('Ctrl Pts',(8.06190272035554,126.999911911841,-106.879456205747));
#25428=CARTESIAN_POINT('Ctrl Pts',(8.06276368953774,126.999898173663,-106.880305951649));
#25429=CARTESIAN_POINT('Ctrl Pts',(8.0635453863377,126.999885700406,-106.881077458535));
#25430=CARTESIAN_POINT('Ctrl Pts',(8.06430194529093,126.999872502733,-106.881824182407));
#25431=CARTESIAN_POINT('Ctrl Pts',(8.0650543196552,126.99985834212,-106.882566882106));
#25432=CARTESIAN_POINT('Ctrl Pts',(8.06584139005466,126.999843528486,-106.883343831688));
#25433=CARTESIAN_POINT('Ctrl Pts',(8.06663114248294,126.99982752742,-106.884123555725));
#25434=CARTESIAN_POINT('Ctrl Pts',(8.06744857778991,126.999809694323,-106.884930805546));
#25435=CARTESIAN_POINT('Ctrl Pts',(8.06836116754174,126.999789785345,-106.885832024159));
#25436=CARTESIAN_POINT('Ctrl Pts',(8.0693076969708,126.999767552881,-106.886766994258));
#25437=CARTESIAN_POINT('Ctrl Pts',(8.07026957515425,126.999743173977,-106.887717360153));
#25438=CARTESIAN_POINT('Ctrl Pts',(8.07152702838454,126.999711303692,-106.88895976349));
#25439=CARTESIAN_POINT('Ctrl Pts',(8.07280899115145,126.999675666215,-106.890226781884));
#25440=CARTESIAN_POINT('Ctrl Pts',(8.07400060096861,126.999639900926,-106.891404811947));
#25441=CARTESIAN_POINT('Ctrl Pts',(8.07497445648938,126.999610671372,-106.892367569273));
#25442=CARTESIAN_POINT('Ctrl Pts',(8.07588470186807,126.999581516183,-106.89326766131));
#25443=CARTESIAN_POINT('Ctrl Pts',(8.0766709110366,126.999555290461,-106.894045268387));
#25444=CARTESIAN_POINT('Ctrl Pts',(8.07735551371743,126.999532454045,-106.894722380676));
#25445=CARTESIAN_POINT('Ctrl Pts',(8.07794516344381,126.999511912239,-106.89530572416));
#25446=CARTESIAN_POINT('Ctrl Pts',(8.07842441386779,126.999494873465,-106.895779966796));
#25447=CARTESIAN_POINT('Ctrl Pts',(8.07886737952789,126.999479124722,-106.896218303816));
#25448=CARTESIAN_POINT('Ctrl Pts',(8.07921553294167,126.999466401456,-106.896562942425));
#25449=CARTESIAN_POINT('Ctrl Pts',(8.07948815114815,126.999456345864,-106.896832907366));
#25450=CARTESIAN_POINT('Ctrl Pts',(8.07974143577804,126.999447003396,-106.897083726895));
#25451=CARTESIAN_POINT('Ctrl Pts',(8.07992930139156,126.999439970325,-106.897269873313));
#25452=CARTESIAN_POINT('Ctrl Pts',(8.08010016396172,126.999433537031,-106.897439207678));
#25453=CARTESIAN_POINT('Ctrl Pts',(8.08013346942631,126.999432283018,-106.897472215257));
#25454=CARTESIAN_POINT('Ctrl Pts',(8.08016624124731,126.999431047035,-106.897504695247));
#25455=CARTESIAN_POINT('Ctrl Pts',(8.08019900800235,126.999429809249,-106.897537170301));
#25456=CARTESIAN_POINT('',(7.7975371703006,126.999429809249,-107.180199008002));
#25457=CARTESIAN_POINT('Ctrl Pts',(7.7975371703006,126.999429809249,-107.180199008002));
#25458=CARTESIAN_POINT('Ctrl Pts',(7.89175778286785,126.999429809249,-107.085978395435));
#25459=CARTESIAN_POINT('Ctrl Pts',(7.9859783954351,126.999429809249,-106.991757782868));
#25460=CARTESIAN_POINT('Ctrl Pts',(8.08019900800235,126.999429809249,-106.897537170301));
#25461=CARTESIAN_POINT('',(7.76770593974857,127.,-107.15));
#25462=CARTESIAN_POINT('Ctrl Pts',(7.7975371703006,126.999429809249,-107.180199008002));
#25463=CARTESIAN_POINT('Ctrl Pts',(7.7973702471606,126.999436171524,-107.180030585505));
#25464=CARTESIAN_POINT('Ctrl Pts',(7.79720010714892,126.999442617638,-107.179858909386));
#25465=CARTESIAN_POINT('Ctrl Pts',(7.79697146331107,126.99945117313,-107.179628057339));
#25466=CARTESIAN_POINT('Ctrl Pts',(7.79671912590221,126.999460615197,-107.179373282892));
#25467=CARTESIAN_POINT('Ctrl Pts',(7.79639560212622,126.999472627869,-107.179046504163));
#25468=CARTESIAN_POINT('Ctrl Pts',(7.79597354340904,126.999487894907,-107.178620026165));
#25469=CARTESIAN_POINT('Ctrl Pts',(7.79550218532651,126.999504945239,-107.1781437326));
#25470=CARTESIAN_POINT('Ctrl Pts',(7.79490840015591,126.999526020176,-107.177543563761));
#25471=CARTESIAN_POINT('Ctrl Pts',(7.79420602224097,126.999549852402,-107.176833440411));
#25472=CARTESIAN_POINT('Ctrl Pts',(7.79331766892345,126.999579994917,-107.175935290825));
#25473=CARTESIAN_POINT('Ctrl Pts',(7.79225701215115,126.999614390365,-107.1748626695));
#25474=CARTESIAN_POINT('Ctrl Pts',(7.7911193310075,126.999648516201,-107.173711822739));
#25475=CARTESIAN_POINT('Ctrl Pts',(7.78997111967503,126.9996829579,-107.17255032393));
#25476=CARTESIAN_POINT('Ctrl Pts',(7.78874985538896,126.999716919438,-107.171314608223));
#25477=CARTESIAN_POINT('Ctrl Pts',(7.78755488645297,126.999747324912,-107.17010513109));
#25478=CARTESIAN_POINT('Ctrl Pts',(7.78666002174368,126.999770094362,-107.169199401769));
#25479=CARTESIAN_POINT('Ctrl Pts',(7.78578043150578,126.999790925398,-107.168308923963));
#25480=CARTESIAN_POINT('Ctrl Pts',(7.78493051996893,126.999809700632,-107.167448288609));
#25481=CARTESIAN_POINT('Ctrl Pts',(7.78415885587109,126.999826747316,-107.166666887987));
#25482=CARTESIAN_POINT('Ctrl Pts',(7.78341204807995,126.999842123653,-107.165910483895));
#25483=CARTESIAN_POINT('Ctrl Pts',(7.78266933990444,126.999856381896,-107.165158111389));
#25484=CARTESIAN_POINT('Ctrl Pts',(7.78189239180835,126.999871297464,-107.164371053423));
#25485=CARTESIAN_POINT('Ctrl Pts',(7.78111275162114,126.999885130105,-107.163581145576));
#25486=CARTESIAN_POINT('Ctrl Pts',(7.78030566598552,126.999898178281,-107.162763400101));
#25487=CARTESIAN_POINT('Ctrl Pts',(7.77940461934248,126.999912745528,-107.161850452599));
#25488=CARTESIAN_POINT('Ctrl Pts',(7.77846992011515,126.999926273619,-107.160903370179));
#25489=CARTESIAN_POINT('Ctrl Pts',(7.77751989647463,126.999938235568,-107.159940788541));
#25490=CARTESIAN_POINT('Ctrl Pts',(7.77627787339686,126.999953874144,-107.158682347638));
#25491=CARTESIAN_POINT('Ctrl Pts',(7.77501135352116,126.999966671765,-107.15739913427));
#25492=CARTESIAN_POINT('Ctrl Pts',(7.77383386704725,126.999975926382,-107.156206223436));
#25493=CARTESIAN_POINT('Ctrl Pts',(7.77287167511962,126.999983488862,-107.155231427377));
#25494=CARTESIAN_POINT('Ctrl Pts',(7.771972161625,126.999988722094,-107.154320197339));
#25495=CARTESIAN_POINT('Ctrl Pts',(7.77119508418426,126.999992198348,-107.153533069771));
#25496=CARTESIAN_POINT('Ctrl Pts',(7.77051841529733,126.999995225425,-107.152847649364));
#25497=CARTESIAN_POINT('Ctrl Pts',(7.76993548245859,126.999996959481,-107.152257239457));
#25498=CARTESIAN_POINT('Ctrl Pts',(7.76946159576003,126.999998025673,-107.15177733498));
#25499=CARTESIAN_POINT('Ctrl Pts',(7.7690235843034,126.999999011149,-107.151333761317));
#25500=CARTESIAN_POINT('Ctrl Pts',(7.76867922569782,126.999999440092,-107.150985093111));
#25501=CARTESIAN_POINT('Ctrl Pts',(7.76840949787861,126.999999683121,-107.150712044098));
#25502=CARTESIAN_POINT('Ctrl Pts',(7.76815889717565,126.999999908916,-107.150458357716));
#25503=CARTESIAN_POINT('Ctrl Pts',(7.76797293322885,126.999999972695,-107.150270163797));
#25504=CARTESIAN_POINT('Ctrl Pts',(7.76780376677657,126.999999993876,-107.150098987781));
#25505=CARTESIAN_POINT('Ctrl Pts',(7.76777080500488,126.999999998003,-107.150065634449));
#25506=CARTESIAN_POINT('Ctrl Pts',(7.76773836991385,127.,-107.15003281473));
#25507=CARTESIAN_POINT('Ctrl Pts',(7.76770593974857,127.,-107.15));
#25508=CARTESIAN_POINT('',(7.90885296987428,127.,-107.008852969874));
#25509=CARTESIAN_POINT('Ctrl Pts',(7.7975371703006,126.999429809249,-107.180199008002));
#25510=CARTESIAN_POINT('Ctrl Pts',(7.99344912464694,126.991962625601,-107.377870706314));
#25511=CARTESIAN_POINT('Ctrl Pts',(8.32585953691074,126.852169925683,-107.68913127501));
#25512=CARTESIAN_POINT('Ctrl Pts',(8.60391850229334,126.49779073068,-107.916788359609));
#25513=CARTESIAN_POINT('Ctrl Pts',(8.65,126.297687701072,-107.95));
#25514=CARTESIAN_POINT('Ctrl Pts',(8.64999999999999,126.2,-107.95));
#25515=CARTESIAN_POINT('Ctrl Pts',(7.89175778286785,126.999429809249,-107.085978395435));
#25516=CARTESIAN_POINT('Ctrl Pts',(8.08825631853607,126.991962625601,-107.283063512425));
#25517=CARTESIAN_POINT('Ctrl Pts',(8.413616782944,126.852169925683,-107.601374028977));
#25518=CARTESIAN_POINT('Ctrl Pts',(8.6748751213987,126.49779073068,-107.845831740504));
#25519=CARTESIAN_POINT('Ctrl Pts',(8.71666666666666,126.297687701072,-107.883333333333));
#25520=CARTESIAN_POINT('Ctrl Pts',(8.71666666666666,126.2,-107.883333333333));
#25521=CARTESIAN_POINT('Ctrl Pts',(7.9859783954351,126.999429809249,-106.991757782868));
#25522=CARTESIAN_POINT('Ctrl Pts',(8.18306351242521,126.991962625601,-107.188256318536));
#25523=CARTESIAN_POINT('Ctrl Pts',(8.50137402897724,126.852169925683,-107.513616782944));
#25524=CARTESIAN_POINT('Ctrl Pts',(8.74583174050407,126.49779073068,-107.774875121399));
#25525=CARTESIAN_POINT('Ctrl Pts',(8.78333333333333,126.297687701072,-107.816666666667));
#25526=CARTESIAN_POINT('Ctrl Pts',(8.78333333333333,126.2,-107.816666666667));
#25527=CARTESIAN_POINT('Ctrl Pts',(8.08019900800235,126.999429809249,-106.897537170301));
#25528=CARTESIAN_POINT('Ctrl Pts',(8.27787070631435,126.991962625601,-107.093449124647));
#25529=CARTESIAN_POINT('Ctrl Pts',(8.58913127501049,126.852169925683,-107.425859536911));
#25530=CARTESIAN_POINT('Ctrl Pts',(8.81678835960943,126.49779073068,-107.703918502293));
#25531=CARTESIAN_POINT('Ctrl Pts',(8.85,126.297687701072,-107.75));
#25532=CARTESIAN_POINT('Ctrl Pts',(8.85,126.2,-107.75));
#25533=CARTESIAN_POINT('',(8.85,126.2,-107.75));
#25534=CARTESIAN_POINT('Ctrl Pts',(8.08019900800235,126.999429809249,-106.897537170301));
#25535=CARTESIAN_POINT('Ctrl Pts',(8.27787070631435,126.991962625601,-107.093449124647));
#25536=CARTESIAN_POINT('Ctrl Pts',(8.58913127501049,126.852169925683,-107.425859536911));
#25537=CARTESIAN_POINT('Ctrl Pts',(8.81678835960943,126.49779073068,-107.703918502293));
#25538=CARTESIAN_POINT('Ctrl Pts',(8.85,126.297687701072,-107.75));
#25539=CARTESIAN_POINT('Ctrl Pts',(8.85,126.2,-107.75));
#25540=CARTESIAN_POINT('',(8.64999999999999,126.2,-107.95));
#25541=CARTESIAN_POINT('',(8.85,126.2,-107.75));
#25542=CARTESIAN_POINT('Ctrl Pts',(8.64999999999999,126.2,-107.95));
#25543=CARTESIAN_POINT('Ctrl Pts',(8.65,126.297687701072,-107.95));
#25544=CARTESIAN_POINT('Ctrl Pts',(8.60391850229334,126.49779073068,-107.916788359609));
#25545=CARTESIAN_POINT('Ctrl Pts',(8.32585953691074,126.852169925683,-107.68913127501));
#25546=CARTESIAN_POINT('Ctrl Pts',(7.99344912464694,126.991962625601,-107.377870706314));
#25547=CARTESIAN_POINT('Ctrl Pts',(7.7975371703006,126.999429809249,-107.180199008002));
#25548=CARTESIAN_POINT('Origin',(8.74999999999999,122.2375,-107.85));
#25549=CARTESIAN_POINT('',(8.84999999999999,123.0375,-107.75));
#25550=CARTESIAN_POINT('',(8.84999999999999,122.2375,-107.75));
#25551=CARTESIAN_POINT('',(8.64999999999999,123.0375,-107.95));
#25552=CARTESIAN_POINT('',(8.84999999999999,123.0375,-107.75));
#25553=CARTESIAN_POINT('',(8.64999999999999,122.2375,-107.95));
#25554=CARTESIAN_POINT('Ctrl Pts',(8.08019900800234,122.238070190751,-106.897537170301));
#25555=CARTESIAN_POINT('Ctrl Pts',(8.27787070631434,122.245537374399,-107.093449124647));
#25556=CARTESIAN_POINT('Ctrl Pts',(8.5891310580126,122.38533016425,-107.425859112781));
#25557=CARTESIAN_POINT('Ctrl Pts',(8.81678792114121,122.739709845598,-107.703918071875));
#25558=CARTESIAN_POINT('Ctrl Pts',(8.85,122.939812298928,-107.75));
#25559=CARTESIAN_POINT('Ctrl Pts',(8.85,123.0375,-107.75));
#25560=CARTESIAN_POINT('Ctrl Pts',(7.98597839543508,122.238070190751,-106.991757782868));
#25561=CARTESIAN_POINT('Ctrl Pts',(8.18306351242519,122.245537374399,-107.188256318536));
#25562=CARTESIAN_POINT('Ctrl Pts',(8.50137374293551,122.38533016425,-107.513616427858));
#25563=CARTESIAN_POINT('Ctrl Pts',(8.74583130471913,122.739709845598,-107.774874688297));
#25564=CARTESIAN_POINT('Ctrl Pts',(8.78333333333333,122.939812298928,-107.816666666667));
#25565=CARTESIAN_POINT('Ctrl Pts',(8.78333333333333,123.0375,-107.816666666667));
#25566=CARTESIAN_POINT('Ctrl Pts',(7.89175778286783,122.238070190751,-107.085978395435));
#25567=CARTESIAN_POINT('Ctrl Pts',(8.08825631853605,122.245537374399,-107.283063512425));
#25568=CARTESIAN_POINT('Ctrl Pts',(8.41361642785841,122.38533016425,-107.601373742935));
#25569=CARTESIAN_POINT('Ctrl Pts',(8.67487468829706,122.739709845598,-107.845831304719));
#25570=CARTESIAN_POINT('Ctrl Pts',(8.71666666666666,122.939812298928,-107.883333333333));
#25571=CARTESIAN_POINT('Ctrl Pts',(8.71666666666666,123.0375,-107.883333333333));
#25572=CARTESIAN_POINT('Ctrl Pts',(7.79753717030057,122.238070190751,-107.180199008002));
#25573=CARTESIAN_POINT('Ctrl Pts',(7.99344912464692,122.245537374399,-107.377870706314));
#25574=CARTESIAN_POINT('Ctrl Pts',(8.32585911278131,122.38533016425,-107.689131058013));
#25575=CARTESIAN_POINT('Ctrl Pts',(8.60391807187497,122.739709845598,-107.916787921141));
#25576=CARTESIAN_POINT('Ctrl Pts',(8.65,122.939812298928,-107.95));
#25577=CARTESIAN_POINT('Ctrl Pts',(8.65,123.0375,-107.95));
#25578=CARTESIAN_POINT('Ctrl Pts',(7.79753717030057,122.238070190751,-107.180199008002));
#25579=CARTESIAN_POINT('Ctrl Pts',(7.99344912464692,122.245537374399,-107.377870706314));
#25580=CARTESIAN_POINT('Ctrl Pts',(8.32585911278131,122.38533016425,-107.689131058013));
#25581=CARTESIAN_POINT('Ctrl Pts',(8.60391807187497,122.739709845598,-107.916787921141));
#25582=CARTESIAN_POINT('Ctrl Pts',(8.65,122.939812298928,-107.95));
#25583=CARTESIAN_POINT('Ctrl Pts',(8.65,123.0375,-107.95));
#25584=CARTESIAN_POINT('Ctrl Pts',(8.85,123.0375,-107.75));
#25585=CARTESIAN_POINT('Ctrl Pts',(8.85,122.939812298928,-107.75));
#25586=CARTESIAN_POINT('Ctrl Pts',(8.81678792114121,122.739709845598,-107.703918071875));
#25587=CARTESIAN_POINT('Ctrl Pts',(8.5891310580126,122.38533016425,-107.425859112781));
#25588=CARTESIAN_POINT('Ctrl Pts',(8.27787070631434,122.245537374399,-107.093449124647));
#25589=CARTESIAN_POINT('Ctrl Pts',(8.08019900800234,122.238070190751,-106.897537170301));
#25590=CARTESIAN_POINT('Origin',(8.05,123.0375,6.35000000000001));
#25591=CARTESIAN_POINT('',(8.84999999999999,123.0375,44.25));
#25592=CARTESIAN_POINT('',(8.84999999999999,123.0375,6.35000000000001));
#25593=CARTESIAN_POINT('',(8.08019900800235,122.238070190751,43.3975371703006));
#25594=CARTESIAN_POINT('Ctrl Pts',(8.08019900800235,122.238070190751,43.3975371703006));
#25595=CARTESIAN_POINT('Ctrl Pts',(8.27787070631434,122.245537374399,43.5934491246469));
#25596=CARTESIAN_POINT('Ctrl Pts',(8.5891258667193,122.385332034808,43.9258486625008));
#25597=CARTESIAN_POINT('Ctrl Pts',(8.81677690192765,122.739724420659,44.2039073549789));
#25598=CARTESIAN_POINT('Ctrl Pts',(8.85,122.939812298928,44.25));
#25599=CARTESIAN_POINT('Ctrl Pts',(8.85,123.0375,44.25));
#25600=CARTESIAN_POINT('Ctrl Pts',(8.05,122.2375,43.3677059397486));
#25601=CARTESIAN_POINT('Ctrl Pts',(8.050168736525,122.2375,43.3678726988052));
#25602=CARTESIAN_POINT('Ctrl Pts',(8.05034072947523,122.237500039141,43.3680426727623));
#25603=CARTESIAN_POINT('Ctrl Pts',(8.05057196841782,122.237500204467,43.3682711198522));
#25604=CARTESIAN_POINT('Ctrl Pts',(8.0508271691041,122.237500386926,43.3685232393849));
#25605=CARTESIAN_POINT('Ctrl Pts',(8.05115445911008,122.23750071898,43.3688465074852));
#25606=CARTESIAN_POINT('Ctrl Pts',(8.05158155127172,122.237501563317,43.3692682628933));
#25607=CARTESIAN_POINT('Ctrl Pts',(8.05205852766469,122.237502506272,43.3697392792016));
#25608=CARTESIAN_POINT('Ctrl Pts',(8.05265950495136,122.237504104656,43.3703326618206));
#25609=CARTESIAN_POINT('Ctrl Pts',(8.05337050733524,122.237507100231,43.3710345962128));
#25610=CARTESIAN_POINT('Ctrl Pts',(8.05426973631202,122.237510888837,43.371922356591));
#25611=CARTESIAN_POINT('Ctrl Pts',(8.05534353223261,122.237517016609,43.3729823430601));
#25612=CARTESIAN_POINT('Ctrl Pts',(8.05649547184038,122.237526369906,43.3741193736361));
#25613=CARTESIAN_POINT('Ctrl Pts',(8.05765817083703,122.237535810566,43.375267024347));
#25614=CARTESIAN_POINT('Ctrl Pts',(8.05889500979368,122.237548536479,43.3764877640867));
#25615=CARTESIAN_POINT('Ctrl Pts',(8.06010536276272,122.237563826519,43.3776823234139));
#25616=CARTESIAN_POINT('Ctrl Pts',(8.06101173564243,122.237575276466,43.3785768692241));
#25617=CARTESIAN_POINT('Ctrl Pts',(8.06190272035532,122.237588088159,43.3794562057464));
#25618=CARTESIAN_POINT('Ctrl Pts',(8.0627636895375,122.237601826337,43.3803059516487));
#25619=CARTESIAN_POINT('Ctrl Pts',(8.06354538633161,122.237614299594,43.3810774585288));
#25620=CARTESIAN_POINT('Ctrl Pts',(8.06430194527942,122.237627497267,43.3818241823961));
#25621=CARTESIAN_POINT('Ctrl Pts',(8.06505431963808,122.237641657879,43.3825668820889));
#25622=CARTESIAN_POINT('Ctrl Pts',(8.06584139003716,122.237656471514,43.3833438316712));
#25623=CARTESIAN_POINT('Ctrl Pts',(8.06663114246472,122.23767247258,43.3841235557071));
#25624=CARTESIAN_POINT('Ctrl Pts',(8.06744857777091,122.237690305677,43.3849308055274));
#25625=CARTESIAN_POINT('Ctrl Pts',(8.06836116752135,122.237710214654,43.3858320241394));
#25626=CARTESIAN_POINT('Ctrl Pts',(8.06930769694889,122.237732447118,43.3867669942366));
#25627=CARTESIAN_POINT('Ctrl Pts',(8.07026957513112,122.237756826022,43.3877173601304));
#25628=CARTESIAN_POINT('Ctrl Pts',(8.07152702835507,122.237788696307,43.3889597634607));
#25629=CARTESIAN_POINT('Ctrl Pts',(8.07280899111595,122.237824333784,43.3902267818492));
#25630=CARTESIAN_POINT('Ctrl Pts',(8.07400060092939,122.237860099073,43.3914048119085));
#25631=CARTESIAN_POINT('Ctrl Pts',(8.07497445645421,122.237889328627,43.3923675692379));
#25632=CARTESIAN_POINT('Ctrl Pts',(8.07588470183759,122.237918483816,43.3932676612799));
#25633=CARTESIAN_POINT('Ctrl Pts',(8.07667091101072,122.237944709538,43.3940452683617));
#25634=CARTESIAN_POINT('Ctrl Pts',(8.0773555136947,122.237967545954,43.3947223806538));
#25635=CARTESIAN_POINT('Ctrl Pts',(8.0779451634244,122.237988087761,43.3953057241405));
#25636=CARTESIAN_POINT('Ctrl Pts',(8.0784244138514,122.238005126535,43.3957799667801));
#25637=CARTESIAN_POINT('Ctrl Pts',(8.07886737951421,122.238020875278,43.3962183038026));
#25638=CARTESIAN_POINT('Ctrl Pts',(8.0792155329305,122.238033598544,43.3965629424142));
#25639=CARTESIAN_POINT('Ctrl Pts',(8.07948815113889,122.238043654136,43.3968329073569));
#25640=CARTESIAN_POINT('Ctrl Pts',(8.07974143577039,122.238052996604,43.3970837268874));
#25641=CARTESIAN_POINT('Ctrl Pts',(8.0799293013851,122.238060029674,43.3972698733071));
#25642=CARTESIAN_POINT('Ctrl Pts',(8.08010016395565,122.238066462969,43.3974392076721));
#25643=CARTESIAN_POINT('Ctrl Pts',(8.08013346942233,122.238067716982,43.3974722152526));
#25644=CARTESIAN_POINT('Ctrl Pts',(8.08016624124532,122.238068952964,43.3975046952449));
#25645=CARTESIAN_POINT('Ctrl Pts',(8.08019900800235,122.238070190751,43.3975371703006));
#25646=CARTESIAN_POINT('Origin',(8.84999999999999,122.2375,44.45));
#25647=CARTESIAN_POINT('',(8.85,126.2,44.25));
#25648=CARTESIAN_POINT('',(8.84999999999999,126.2,6.35000000000001));
#25649=CARTESIAN_POINT('',(8.84999999999999,122.2375,44.25));
#25650=CARTESIAN_POINT('Origin',(8.05,126.2,6.35000000000001));
#25651=CARTESIAN_POINT('',(8.05,127.,43.3677059397486));
#25652=CARTESIAN_POINT('',(8.05,127.,6.35000000000001));
#25653=CARTESIAN_POINT('',(8.08019900800234,126.999429809249,43.3975371703006));
#25654=CARTESIAN_POINT('Ctrl Pts',(8.08019900800234,126.999429809249,43.3975371703006));
#25655=CARTESIAN_POINT('Ctrl Pts',(8.0800305855052,126.999436171524,43.3973702471606));
#25656=CARTESIAN_POINT('Ctrl Pts',(8.0798589093858,126.999442617638,43.3972001071489));
#25657=CARTESIAN_POINT('Ctrl Pts',(8.07962805733889,126.99945117313,43.3969714633111));
#25658=CARTESIAN_POINT('Ctrl Pts',(8.0793732828919,126.999460615197,43.3967191259022));
#25659=CARTESIAN_POINT('Ctrl Pts',(8.07904650416285,126.999472627869,43.3963956021262));
#25660=CARTESIAN_POINT('Ctrl Pts',(8.0786200261654,126.999487894907,43.395973543409));
#25661=CARTESIAN_POINT('Ctrl Pts',(8.07814373260023,126.999504945239,43.3955021853265));
#25662=CARTESIAN_POINT('Ctrl Pts',(8.07754356376057,126.999526020176,43.3949084001559));
#25663=CARTESIAN_POINT('Ctrl Pts',(8.07683344041104,126.999549852402,43.3942060222409));
#25664=CARTESIAN_POINT('Ctrl Pts',(8.07593529082521,126.999579994917,43.3933176689234));
#25665=CARTESIAN_POINT('Ctrl Pts',(8.07486266949977,126.999614390365,43.3922570121511));
#25666=CARTESIAN_POINT('Ctrl Pts',(8.07371182273854,126.999648516201,43.3911193310075));
#25667=CARTESIAN_POINT('Ctrl Pts',(8.07255032392972,126.9996829579,43.389971119675));
#25668=CARTESIAN_POINT('Ctrl Pts',(8.07131460822261,126.999716919438,43.3887498553889));
#25669=CARTESIAN_POINT('Ctrl Pts',(8.07010513108995,126.999747324912,43.3875548864529));
#25670=CARTESIAN_POINT('Ctrl Pts',(8.06919940176919,126.999770094362,43.3866600217436));
#25671=CARTESIAN_POINT('Ctrl Pts',(8.06830892396286,126.999790925398,43.3857804315057));
#25672=CARTESIAN_POINT('Ctrl Pts',(8.06744828860937,126.999809700632,43.3849305199689));
#25673=CARTESIAN_POINT('Ctrl Pts',(8.06666688798462,126.999826747316,43.3841588558684));
#25674=CARTESIAN_POINT('Ctrl Pts',(8.06591048388973,126.999842123653,43.3834120480748));
#25675=CARTESIAN_POINT('Ctrl Pts',(8.06515811138141,126.999856381896,43.3826693398968));
#25676=CARTESIAN_POINT('Ctrl Pts',(8.06437105341527,126.999871297464,43.3818923918005));
#25677=CARTESIAN_POINT('Ctrl Pts',(8.0635811455681,126.999885130105,43.381112751613));
#25678=CARTESIAN_POINT('Ctrl Pts',(8.06276340009277,126.999898178282,43.380305665977));
#25679=CARTESIAN_POINT('Ctrl Pts',(8.06185045258994,126.999912745528,43.3794046193334));
#25680=CARTESIAN_POINT('Ctrl Pts',(8.06090337016919,126.999926273619,43.3784699201053));
#25681=CARTESIAN_POINT('Ctrl Pts',(8.0599407885309,126.999938235568,43.3775198964643));
#25682=CARTESIAN_POINT('Ctrl Pts',(8.05868234762488,126.999953874144,43.3762778733838));
#25683=CARTESIAN_POINT('Ctrl Pts',(8.05739913425408,126.999966671765,43.3750113535055));
#25684=CARTESIAN_POINT('Ctrl Pts',(8.05620622341898,126.999975926382,43.37383386703));
#25685=CARTESIAN_POINT('Ctrl Pts',(8.05523142736173,126.999983488862,43.3728716751042));
#25686=CARTESIAN_POINT('Ctrl Pts',(8.05432019732505,126.999988722094,43.3719721616116));
#25687=CARTESIAN_POINT('Ctrl Pts',(8.05353306975903,126.999992198348,43.3711950841729));
#25688=CARTESIAN_POINT('Ctrl Pts',(8.05284764935386,126.999995225425,43.3705184152873));
#25689=CARTESIAN_POINT('Ctrl Pts',(8.05225723944801,126.999996959481,43.36993548245));
#25690=CARTESIAN_POINT('Ctrl Pts',(8.05177733497262,126.999998025673,43.3694615957528));
#25691=CARTESIAN_POINT('Ctrl Pts',(8.05133376131042,126.999999011149,43.3690235842973));
#25692=CARTESIAN_POINT('Ctrl Pts',(8.0509850931062,126.999999440092,43.3686792256928));
#25693=CARTESIAN_POINT('Ctrl Pts',(8.05071204409405,126.999999683121,43.3684094978744));
#25694=CARTESIAN_POINT('Ctrl Pts',(8.0504583577127,126.999999908916,43.3681588971722));
#25695=CARTESIAN_POINT('Ctrl Pts',(8.05027016379399,126.999999972695,43.3679729332259));
#25696=CARTESIAN_POINT('Ctrl Pts',(8.05009898777776,126.999999993876,43.3678037667738));
#25697=CARTESIAN_POINT('Ctrl Pts',(8.05006563444715,126.999999998003,43.3677708050031));
#25698=CARTESIAN_POINT('Ctrl Pts',(8.05003281472894,127.,43.3677383699129));
#25699=CARTESIAN_POINT('Ctrl Pts',(8.05,127.,43.3677059397486));
#25700=CARTESIAN_POINT('Ctrl Pts',(8.85,126.2,44.25));
#25701=CARTESIAN_POINT('Ctrl Pts',(8.85,126.297687701072,44.25));
#25702=CARTESIAN_POINT('Ctrl Pts',(8.81677764270249,126.497776564831,44.2039080692991));
#25703=CARTESIAN_POINT('Ctrl Pts',(8.58912619963984,126.852168067061,43.9258493522423));
#25704=CARTESIAN_POINT('Ctrl Pts',(8.27787070631434,126.991962625601,43.5934491246469));
#25705=CARTESIAN_POINT('Ctrl Pts',(8.08019900800234,126.999429809249,43.3975371703006));
#25706=CARTESIAN_POINT('Origin',(-29.25,127.,-31.75));
#25707=CARTESIAN_POINT('',(7.76770593974856,127.,43.65));
#25708=CARTESIAN_POINT('',(-48.3,127.,43.65));
#25709=CARTESIAN_POINT('',(7.90885296987428,127.,43.5088529698743));
#25710=CARTESIAN_POINT('',(-10.2,127.,-107.15));
#25711=CARTESIAN_POINT('Ctrl Pts',(8.08019900800235,122.238070190751,43.3975371703006));
#25712=CARTESIAN_POINT('Ctrl Pts',(8.07851655455606,122.238006634921,43.395869694655));
#25713=CARTESIAN_POINT('Ctrl Pts',(8.06616819355892,122.2375677537,43.3836608980584));
#25714=CARTESIAN_POINT('Ctrl Pts',(8.05260673028965,122.237504057297,43.3702834872759));
#25715=CARTESIAN_POINT('Ctrl Pts',(8.05042140713843,122.2375,43.3681224083044));
#25716=CARTESIAN_POINT('Ctrl Pts',(8.05,122.2375,43.3677059397486));
#25717=CARTESIAN_POINT('Ctrl Pts',(7.98597839543509,122.238070190751,43.4917577828678));
#25718=CARTESIAN_POINT('Ctrl Pts',(7.98430093458904,122.238006634921,43.490085314622));
#25719=CARTESIAN_POINT('Ctrl Pts',(7.97200590495255,122.2375677537,43.4778231866648));
#25720=CARTESIAN_POINT('Ctrl Pts',(7.95849656571179,122.237504057297,43.4643936518537));
#25721=CARTESIAN_POINT('Ctrl Pts',(7.9563217408604,122.2375,43.4622220745824));
#25722=CARTESIAN_POINT('Ctrl Pts',(7.95590197991618,122.2375,43.4618039598324));
#25723=CARTESIAN_POINT('Ctrl Pts',(7.89175778286784,122.238070190751,43.5859783954351));
#25724=CARTESIAN_POINT('Ctrl Pts',(7.89008531462202,122.238006634921,43.584300934589));
#25725=CARTESIAN_POINT('Ctrl Pts',(7.87782318666485,122.237493013703,43.5719650959653));
#25726=CARTESIAN_POINT('Ctrl Pts',(7.8643936518537,122.237549698229,43.5584909077319));
#25727=CARTESIAN_POINT('Ctrl Pts',(7.86222207458237,122.2375,43.5563217408604));
#25728=CARTESIAN_POINT('Ctrl Pts',(7.86180395983237,122.2375,43.5559019799162));
#25729=CARTESIAN_POINT('Ctrl Pts',(7.79753717030059,122.238070190751,43.6801990080023));
#25730=CARTESIAN_POINT('Ctrl Pts',(7.795869694655,122.238006634921,43.6785165545561));
#25731=CARTESIAN_POINT('Ctrl Pts',(7.78366089805848,122.2375677537,43.6661681935589));
#25732=CARTESIAN_POINT('Ctrl Pts',(7.77028348727585,122.237504057297,43.6526067302897));
#25733=CARTESIAN_POINT('Ctrl Pts',(7.76812240830434,122.2375,43.6504214071384));
#25734=CARTESIAN_POINT('Ctrl Pts',(7.76770593974856,122.2375,43.65));
#25735=CARTESIAN_POINT('',(7.79753717030059,122.238070190751,43.6801990080023));
#25736=CARTESIAN_POINT('Ctrl Pts',(7.79753717030059,122.238070190751,43.6801990080023));
#25737=CARTESIAN_POINT('Ctrl Pts',(7.89175778286784,122.238070190751,43.5859783954351));
#25738=CARTESIAN_POINT('Ctrl Pts',(7.98597839543509,122.238070190751,43.4917577828678));
#25739=CARTESIAN_POINT('Ctrl Pts',(8.08019900800235,122.238070190751,43.3975371703006));
#25740=CARTESIAN_POINT('Ctrl Pts',(7.79753717030059,122.238070190751,43.6801990080023));
#25741=CARTESIAN_POINT('Ctrl Pts',(7.79737024716059,122.238063828476,43.6800305855052));
#25742=CARTESIAN_POINT('Ctrl Pts',(7.79720010714893,122.238057382362,43.6798589093858));
#25743=CARTESIAN_POINT('Ctrl Pts',(7.79697146331107,122.23804882687,43.6796280573389));
#25744=CARTESIAN_POINT('Ctrl Pts',(7.79671912590222,122.238039384803,43.6793732828919));
#25745=CARTESIAN_POINT('Ctrl Pts',(7.79639560212623,122.238027372131,43.6790465041629));
#25746=CARTESIAN_POINT('Ctrl Pts',(7.79597354340905,122.238012105093,43.6786200261654));
#25747=CARTESIAN_POINT('Ctrl Pts',(7.79550218532653,122.237995054761,43.6781437326003));
#25748=CARTESIAN_POINT('Ctrl Pts',(7.79490840015591,122.237973979824,43.6775435637606));
#25749=CARTESIAN_POINT('Ctrl Pts',(7.79420602224099,122.237950147598,43.6768334404111));
#25750=CARTESIAN_POINT('Ctrl Pts',(7.79331766892344,122.237920005083,43.6759352908252));
#25751=CARTESIAN_POINT('Ctrl Pts',(7.79225701215112,122.237885609635,43.6748626694998));
#25752=CARTESIAN_POINT('Ctrl Pts',(7.79111933100742,122.237851483799,43.6737118227385));
#25753=CARTESIAN_POINT('Ctrl Pts',(7.78997111967495,122.2378170421,43.6725503239297));
#25754=CARTESIAN_POINT('Ctrl Pts',(7.78874985538888,122.237783080562,43.6713146082226));
#25755=CARTESIAN_POINT('Ctrl Pts',(7.7875548864529,122.237752675088,43.6701051310899));
#25756=CARTESIAN_POINT('Ctrl Pts',(7.78666002174363,122.237729905638,43.6691994017692));
#25757=CARTESIAN_POINT('Ctrl Pts',(7.78578043150577,122.237709074602,43.6683089239629));
#25758=CARTESIAN_POINT('Ctrl Pts',(7.78493051996895,122.237690299368,43.6674482886095));
#25759=CARTESIAN_POINT('Ctrl Pts',(7.78415885587012,122.237673252684,43.6666668879864));
#25760=CARTESIAN_POINT('Ctrl Pts',(7.78341204807806,122.237657876347,43.665910483893));
#25761=CARTESIAN_POINT('Ctrl Pts',(7.7826693399016,122.237643618104,43.6651581113863));
#25762=CARTESIAN_POINT('Ctrl Pts',(7.78189239180545,122.237628702536,43.6643710534202));
#25763=CARTESIAN_POINT('Ctrl Pts',(7.78111275161813,122.237614869895,43.6635811455733));
#25764=CARTESIAN_POINT('Ctrl Pts',(7.78030566598238,122.237601821719,43.6627634000982));
#25765=CARTESIAN_POINT('Ctrl Pts',(7.77940461933911,122.237587254472,43.6618504525958));
#25766=CARTESIAN_POINT('Ctrl Pts',(7.77846992011155,122.237573726381,43.6609033701755));
#25767=CARTESIAN_POINT('Ctrl Pts',(7.77751989647083,122.237561764432,43.6599407885375));
#25768=CARTESIAN_POINT('Ctrl Pts',(7.77627787339213,122.237546125856,43.6586823476333));
#25769=CARTESIAN_POINT('Ctrl Pts',(7.77501135351555,122.237533328235,43.6573991342643));
#25770=CARTESIAN_POINT('Ctrl Pts',(7.77383386704111,122.237524073618,43.6562062234303));
#25771=CARTESIAN_POINT('Ctrl Pts',(7.77287167511409,122.237516511138,43.6552314273718));
#25772=CARTESIAN_POINT('Ctrl Pts',(7.77197216162022,122.237511277906,43.6543201973338));
#25773=CARTESIAN_POINT('Ctrl Pts',(7.77119508418019,122.237507801652,43.6535330697664));
#25774=CARTESIAN_POINT('Ctrl Pts',(7.77051841529376,122.237504774575,43.6528476493604));
#25775=CARTESIAN_POINT('Ctrl Pts',(7.76993548245554,122.237503040519,43.6522572394536));
#25776=CARTESIAN_POINT('Ctrl Pts',(7.76946159575746,122.237501974327,43.6517773349774));
#25777=CARTESIAN_POINT('Ctrl Pts',(7.76902358430123,122.237500988851,43.6513337613144));
#25778=CARTESIAN_POINT('Ctrl Pts',(7.76867922569604,122.237500559908,43.6509850931095));
#25779=CARTESIAN_POINT('Ctrl Pts',(7.76840949787714,122.237500316879,43.6507120440968));
#25780=CARTESIAN_POINT('Ctrl Pts',(7.76815889717443,122.237500091084,43.650458357715));
#25781=CARTESIAN_POINT('Ctrl Pts',(7.76797293322782,122.237500027304,43.6502701637959));
#25782=CARTESIAN_POINT('Ctrl Pts',(7.76780376677561,122.237500006124,43.6500989877796));
#25783=CARTESIAN_POINT('Ctrl Pts',(7.76777080500425,122.237500001997,43.6500656344483));
#25784=CARTESIAN_POINT('Ctrl Pts',(7.76773836991353,122.2375,43.6500328147295));
#25785=CARTESIAN_POINT('Ctrl Pts',(7.76770593974857,122.2375,43.65));
#25786=CARTESIAN_POINT('Ctrl Pts',(7.79753717030059,126.999429809249,43.6801990080023));
#25787=CARTESIAN_POINT('Ctrl Pts',(7.79586969465498,126.999493365079,43.6785165545561));
#25788=CARTESIAN_POINT('Ctrl Pts',(7.78366122669983,126.999932239882,43.6661685239879));
#25789=CARTESIAN_POINT('Ctrl Pts',(7.77028357183286,126.999995941636,43.6526068154461));
#25790=CARTESIAN_POINT('Ctrl Pts',(7.76812240830435,127.,43.6504214071384));
#25791=CARTESIAN_POINT('Ctrl Pts',(7.76770593974856,127.,43.65));
#25792=CARTESIAN_POINT('Ctrl Pts',(7.89175778286784,126.999429809249,43.5859783954351));
#25793=CARTESIAN_POINT('Ctrl Pts',(7.890085314622,126.999493365079,43.584300934589));
#25794=CARTESIAN_POINT('Ctrl Pts',(7.8778235153062,126.999932239882,43.5720062353815));
#25795=CARTESIAN_POINT('Ctrl Pts',(7.86439373641072,126.999995941636,43.5584966508682));
#25796=CARTESIAN_POINT('Ctrl Pts',(7.86222207458238,127.,43.5563217408604));
#25797=CARTESIAN_POINT('Ctrl Pts',(7.86180395983237,127.,43.5559019799162));
#25798=CARTESIAN_POINT('Ctrl Pts',(7.98597839543509,126.999429809249,43.4917577828678));
#25799=CARTESIAN_POINT('Ctrl Pts',(7.98430093458903,126.999493365079,43.490085314622));
#25800=CARTESIAN_POINT('Ctrl Pts',(7.97196542790919,127.000007018684,43.4778235153062));
#25801=CARTESIAN_POINT('Ctrl Pts',(7.9584909931402,126.999950310709,43.4643937364107));
#25802=CARTESIAN_POINT('Ctrl Pts',(7.9563217408604,127.,43.4622220745824));
#25803=CARTESIAN_POINT('Ctrl Pts',(7.95590197991619,127.,43.4618039598324));
#25804=CARTESIAN_POINT('Ctrl Pts',(8.08019900800234,126.999429809249,43.3975371703006));
#25805=CARTESIAN_POINT('Ctrl Pts',(8.07851655455605,126.999493365079,43.395869694655));
#25806=CARTESIAN_POINT('Ctrl Pts',(8.06616852398783,126.999932239882,43.3836612266998));
#25807=CARTESIAN_POINT('Ctrl Pts',(8.05260681544608,126.999995941636,43.3702835718329));
#25808=CARTESIAN_POINT('Ctrl Pts',(8.05042140713843,127.,43.3681224083043));
#25809=CARTESIAN_POINT('Ctrl Pts',(8.05,127.,43.3677059397486));
#25810=CARTESIAN_POINT('',(7.79753717030059,126.999429809249,43.6801990080023));
#25811=CARTESIAN_POINT('Ctrl Pts',(7.76770593974857,127.,43.65));
#25812=CARTESIAN_POINT('Ctrl Pts',(7.76787269880523,127.,43.650168736525));
#25813=CARTESIAN_POINT('Ctrl Pts',(7.76804267276226,126.999999960859,43.6503407294752));
#25814=CARTESIAN_POINT('Ctrl Pts',(7.76827111985223,126.999999795533,43.6505719684178));
#25815=CARTESIAN_POINT('Ctrl Pts',(7.76852323938489,126.999999613074,43.6508271691041));
#25816=CARTESIAN_POINT('Ctrl Pts',(7.76884650748516,126.99999928102,43.6511544591101));
#25817=CARTESIAN_POINT('Ctrl Pts',(7.76926826289326,126.999998436683,43.6515815512717));
#25818=CARTESIAN_POINT('Ctrl Pts',(7.76973927920159,126.999997493728,43.6520585276647));
#25819=CARTESIAN_POINT('Ctrl Pts',(7.7703326618207,126.999995895344,43.6526595049515));
#25820=CARTESIAN_POINT('Ctrl Pts',(7.77103459621293,126.999992899769,43.6533705073354));
#25821=CARTESIAN_POINT('Ctrl Pts',(7.77192235659121,126.999989111163,43.6542697363123));
#25822=CARTESIAN_POINT('Ctrl Pts',(7.77298234306036,126.999982983391,43.6553435322329));
#25823=CARTESIAN_POINT('Ctrl Pts',(7.7741193736364,126.999973630094,43.6564954718407));
#25824=CARTESIAN_POINT('Ctrl Pts',(7.77526702434735,126.999964189434,43.6576581708374));
#25825=CARTESIAN_POINT('Ctrl Pts',(7.77648776408707,126.999951463521,43.658895009794));
#25826=CARTESIAN_POINT('Ctrl Pts',(7.77768232341421,126.999936173481,43.6601053627631));
#25827=CARTESIAN_POINT('Ctrl Pts',(7.7785768692244,126.999924723534,43.6610117356427));
#25828=CARTESIAN_POINT('Ctrl Pts',(7.77945620574664,126.999911911841,43.6619027203556));
#25829=CARTESIAN_POINT('Ctrl Pts',(7.78030595164888,126.999898173663,43.6627636895377));
#25830=CARTESIAN_POINT('Ctrl Pts',(7.78107745852858,126.999885700406,43.6635453863314));
#25831=CARTESIAN_POINT('Ctrl Pts',(7.78182418239544,126.999872502733,43.6643019452788));
#25832=CARTESIAN_POINT('Ctrl Pts',(7.78256688208792,126.999858342121,43.6650543196371));
#25833=CARTESIAN_POINT('Ctrl Pts',(7.78334383167018,126.999843528486,43.6658413900361));
#25834=CARTESIAN_POINT('Ctrl Pts',(7.78412355570597,126.99982752742,43.6666311424636));
#25835=CARTESIAN_POINT('Ctrl Pts',(7.78493080552624,126.999809694323,43.6674485777698));
#25836=CARTESIAN_POINT('Ctrl Pts',(7.78583202413818,126.999789785346,43.6683611675201));
#25837=CARTESIAN_POINT('Ctrl Pts',(7.78676699423533,126.999767552882,43.6693076969476));
#25838=CARTESIAN_POINT('Ctrl Pts',(7.78771736012898,126.999743173978,43.6702695751297));
#25839=CARTESIAN_POINT('Ctrl Pts',(7.78895976345899,126.999711303693,43.6715270283533));
#25840=CARTESIAN_POINT('Ctrl Pts',(7.79022678184709,126.999675666216,43.6728089911139));
#25841=CARTESIAN_POINT('Ctrl Pts',(7.79140481190622,126.999639900927,43.6740006009271));
#25842=CARTESIAN_POINT('Ctrl Pts',(7.79236756923585,126.999610671373,43.6749744564522));
#25843=CARTESIAN_POINT('Ctrl Pts',(7.79326766127809,126.999581516184,43.6758847018358));
#25844=CARTESIAN_POINT('Ctrl Pts',(7.79404526836015,126.999555290462,43.6766709110092));
#25845=CARTESIAN_POINT('Ctrl Pts',(7.79472238065246,126.999532454046,43.6773555136934));
#25846=CARTESIAN_POINT('Ctrl Pts',(7.79530572413939,126.999511912239,43.6779451634233));
#25847=CARTESIAN_POINT('Ctrl Pts',(7.79577996677921,126.999494873465,43.6784244138505));
#25848=CARTESIAN_POINT('Ctrl Pts',(7.79621830380183,126.999479124722,43.6788673795135));
#25849=CARTESIAN_POINT('Ctrl Pts',(7.79656294241353,126.999466401456,43.6792155329299));
#25850=CARTESIAN_POINT('Ctrl Pts',(7.79683290735634,126.999456345864,43.6794881511384));
#25851=CARTESIAN_POINT('Ctrl Pts',(7.79708372688692,126.999447003396,43.6797414357699));
#25852=CARTESIAN_POINT('Ctrl Pts',(7.7972698733067,126.999439970326,43.6799293013847));
#25853=CARTESIAN_POINT('Ctrl Pts',(7.79743920767177,126.999433537031,43.6801001639553));
#25854=CARTESIAN_POINT('Ctrl Pts',(7.79747221525241,126.999432283018,43.6801334694221));
#25855=CARTESIAN_POINT('Ctrl Pts',(7.79750469524479,126.999431047036,43.6801662412452));
#25856=CARTESIAN_POINT('Ctrl Pts',(7.79753717030059,126.999429809249,43.6801990080023));
#25857=CARTESIAN_POINT('Ctrl Pts',(8.08019900800234,126.999429809249,43.3975371703006));
#25858=CARTESIAN_POINT('Ctrl Pts',(7.98597839543509,126.999429809249,43.4917577828678));
#25859=CARTESIAN_POINT('Ctrl Pts',(7.89175778286784,126.999429809249,43.5859783954351));
#25860=CARTESIAN_POINT('Ctrl Pts',(7.79753717030059,126.999429809249,43.6801990080023));
#25861=CARTESIAN_POINT('Ctrl Pts',(8.08019900800234,126.999429809249,43.3975371703006));
#25862=CARTESIAN_POINT('Ctrl Pts',(8.27787070631434,126.991962625601,43.5934491246469));
#25863=CARTESIAN_POINT('Ctrl Pts',(8.58912619963984,126.852168067061,43.9258493522423));
#25864=CARTESIAN_POINT('Ctrl Pts',(8.81677764270249,126.497776564831,44.2039080692991));
#25865=CARTESIAN_POINT('Ctrl Pts',(8.85,126.297687701072,44.25));
#25866=CARTESIAN_POINT('Ctrl Pts',(8.85,126.2,44.25));
#25867=CARTESIAN_POINT('Ctrl Pts',(7.98597839543509,126.999429809249,43.4917577828678));
#25868=CARTESIAN_POINT('Ctrl Pts',(8.1830635124252,126.991962625601,43.6882563185361));
#25869=CARTESIAN_POINT('Ctrl Pts',(8.50136725050732,126.852168067061,44.0136083013748));
#25870=CARTESIAN_POINT('Ctrl Pts',(8.74582111823467,126.497776564831,44.2748645937669));
#25871=CARTESIAN_POINT('Ctrl Pts',(8.78333333333332,126.297687701072,44.3166666666667));
#25872=CARTESIAN_POINT('Ctrl Pts',(8.78333333333332,126.2,44.3166666666667));
#25873=CARTESIAN_POINT('Ctrl Pts',(7.89175778286784,126.999429809249,43.5859783954351));
#25874=CARTESIAN_POINT('Ctrl Pts',(8.08825631853606,126.991962625601,43.7830635124252));
#25875=CARTESIAN_POINT('Ctrl Pts',(8.41360830137479,126.852168067061,44.1013672505073));
#25876=CARTESIAN_POINT('Ctrl Pts',(8.67486459376686,126.497776564831,44.3458211182347));
#25877=CARTESIAN_POINT('Ctrl Pts',(8.71666666666665,126.297687701072,44.3833333333333));
#25878=CARTESIAN_POINT('Ctrl Pts',(8.71666666666665,126.2,44.3833333333333));
#25879=CARTESIAN_POINT('Ctrl Pts',(7.79753717030059,126.999429809249,43.6801990080023));
#25880=CARTESIAN_POINT('Ctrl Pts',(7.99344912464693,126.991962625601,43.8778707063143));
#25881=CARTESIAN_POINT('Ctrl Pts',(8.32584935224227,126.852168067061,44.1891261996398));
#25882=CARTESIAN_POINT('Ctrl Pts',(8.60390806929905,126.497776564831,44.4167776427025));
#25883=CARTESIAN_POINT('Ctrl Pts',(8.64999999999998,126.297687701072,44.45));
#25884=CARTESIAN_POINT('Ctrl Pts',(8.64999999999998,126.2,44.45));
#25885=CARTESIAN_POINT('',(8.64999999999998,126.2,44.45));
#25886=CARTESIAN_POINT('Ctrl Pts',(7.79753717030059,126.999429809249,43.6801990080023));
#25887=CARTESIAN_POINT('Ctrl Pts',(7.99344912464693,126.991962625601,43.8778707063143));
#25888=CARTESIAN_POINT('Ctrl Pts',(8.32584935224227,126.852168067061,44.1891261996398));
#25889=CARTESIAN_POINT('Ctrl Pts',(8.60390806929905,126.497776564831,44.4167776427025));
#25890=CARTESIAN_POINT('Ctrl Pts',(8.64999999999998,126.297687701072,44.45));
#25891=CARTESIAN_POINT('Ctrl Pts',(8.64999999999998,126.2,44.45));
#25892=CARTESIAN_POINT('',(8.64999999999998,126.2,44.45));
#25893=CARTESIAN_POINT('Origin',(8.74999999999999,122.2375,44.35));
#25894=CARTESIAN_POINT('',(8.64999999999999,123.0375,44.45));
#25895=CARTESIAN_POINT('',(8.64999999999999,122.2375,44.45));
#25896=CARTESIAN_POINT('',(8.64999999999999,123.0375,44.45));
#25897=CARTESIAN_POINT('Ctrl Pts',(7.79753717030059,122.238070190751,43.6801990080023));
#25898=CARTESIAN_POINT('Ctrl Pts',(7.99344912464693,122.245537374399,43.8778707063143));
#25899=CARTESIAN_POINT('Ctrl Pts',(8.3258486625008,122.385332034808,44.1891258667193));
#25900=CARTESIAN_POINT('Ctrl Pts',(8.60390735497882,122.739724420659,44.4167769019277));
#25901=CARTESIAN_POINT('Ctrl Pts',(8.64999999999998,122.939812298928,44.45));
#25902=CARTESIAN_POINT('Ctrl Pts',(8.64999999999998,123.0375,44.45));
#25903=CARTESIAN_POINT('Ctrl Pts',(7.89175778286784,122.238070190751,43.5859783954351));
#25904=CARTESIAN_POINT('Ctrl Pts',(8.08825631853606,122.245537374399,43.7830635124252));
#25905=CARTESIAN_POINT('Ctrl Pts',(8.41360773057363,122.385332034808,44.1013667986465));
#25906=CARTESIAN_POINT('Ctrl Pts',(8.67486387062843,122.739724420659,44.3458203862781));
#25907=CARTESIAN_POINT('Ctrl Pts',(8.71666666666665,122.939812298928,44.3833333333333));
#25908=CARTESIAN_POINT('Ctrl Pts',(8.71666666666665,123.0375,44.3833333333333));
#25909=CARTESIAN_POINT('Ctrl Pts',(7.98597839543509,122.238070190751,43.4917577828678));
#25910=CARTESIAN_POINT('Ctrl Pts',(8.1830635124252,122.245537374399,43.6882563185361));
#25911=CARTESIAN_POINT('Ctrl Pts',(8.50136679864646,122.385332034808,44.0136077305736));
#25912=CARTESIAN_POINT('Ctrl Pts',(8.74582038627804,122.739724420659,44.2748638706285));
#25913=CARTESIAN_POINT('Ctrl Pts',(8.78333333333332,122.939812298928,44.3166666666667));
#25914=CARTESIAN_POINT('Ctrl Pts',(8.78333333333332,123.0375,44.3166666666667));
#25915=CARTESIAN_POINT('Ctrl Pts',(8.08019900800235,122.238070190751,43.3975371703006));
#25916=CARTESIAN_POINT('Ctrl Pts',(8.27787070631434,122.245537374399,43.5934491246469));
#25917=CARTESIAN_POINT('Ctrl Pts',(8.5891258667193,122.385332034808,43.9258486625008));
#25918=CARTESIAN_POINT('Ctrl Pts',(8.81677690192765,122.739724420659,44.2039073549789));
#25919=CARTESIAN_POINT('Ctrl Pts',(8.85,122.939812298928,44.25));
#25920=CARTESIAN_POINT('Ctrl Pts',(8.85,123.0375,44.25));
#25921=CARTESIAN_POINT('Ctrl Pts',(8.64999999999998,123.0375,44.45));
#25922=CARTESIAN_POINT('Ctrl Pts',(8.64999999999998,122.939812298928,44.45));
#25923=CARTESIAN_POINT('Ctrl Pts',(8.60390735497882,122.739724420659,44.4167769019277));
#25924=CARTESIAN_POINT('Ctrl Pts',(8.3258486625008,122.385332034808,44.1891258667193));
#25925=CARTESIAN_POINT('Ctrl Pts',(7.99344912464693,122.245537374399,43.8778707063143));
#25926=CARTESIAN_POINT('Ctrl Pts',(7.79753717030059,122.238070190751,43.6801990080023));
#25927=CARTESIAN_POINT('Origin',(-48.3,123.0375,43.65));
#25928=CARTESIAN_POINT('',(-48.3,123.0375,44.45));
#25929=CARTESIAN_POINT('Origin',(-67.35,122.2375,44.45));
#25930=CARTESIAN_POINT('',(-48.3,126.2,44.45));
#25931=CARTESIAN_POINT('Origin',(-48.3,126.2,43.65));
#25932=CARTESIAN_POINT('Origin',(-10.2,126.2,-107.15));
#25933=CARTESIAN_POINT('',(-10.2,126.2,-107.95));
#25934=CARTESIAN_POINT('Origin',(8.85,122.2375,-107.95));
#25935=CARTESIAN_POINT('',(-10.2,123.0375,-107.95));
#25936=CARTESIAN_POINT('Origin',(-10.2,123.0375,-107.15));
#25937=CARTESIAN_POINT('',(0.,0.,0.));
#25938=CARTESIAN_POINT('Origin',(28.2,-32.15,4.));
#25939=CARTESIAN_POINT('',(34.,-31.9,10.2136945531624));
#25940=CARTESIAN_POINT('',(34.,-32.4,10.8818602136341));
#25941=CARTESIAN_POINT('Ctrl Pts',(34.,-32.4,10.8818602136341));
#25942=CARTESIAN_POINT('Ctrl Pts',(34.,-32.1372444185762,10.5382321596773));
#25943=CARTESIAN_POINT('Ctrl Pts',(34.,-31.9,10.2136945531624));
#25944=CARTESIAN_POINT('',(37.2,-32.4,4.));
#25945=CARTESIAN_POINT('Origin',(28.2,-32.4,4.));
#25946=CARTESIAN_POINT('',(36.7,-31.9,4.));
#25947=CARTESIAN_POINT('',(37.2,-32.4,4.));
#25948=CARTESIAN_POINT('Origin',(28.2,-31.9,4.));
#25949=CARTESIAN_POINT('Origin',(36.95,-32.15,-2.));
#25950=CARTESIAN_POINT('',(37.2,-32.4,-4.));
#25951=CARTESIAN_POINT('',(37.2,-32.4,-2.));
#25952=CARTESIAN_POINT('',(36.7,-31.9,-4.));
#25953=CARTESIAN_POINT('',(37.2,-32.4,-4.));
#25954=CARTESIAN_POINT('',(36.7,-31.9,-2.));
#25955=CARTESIAN_POINT('Origin',(28.2,-32.15,-4.));
#25956=CARTESIAN_POINT('',(34.,-32.4,-10.8818602136341));
#25957=CARTESIAN_POINT('',(34.,-31.9,-10.2136945531624));
#25958=CARTESIAN_POINT('Ctrl Pts',(34.,-31.9,-10.2136945531624));
#25959=CARTESIAN_POINT('Ctrl Pts',(34.,-32.1372444185762,-10.5382321596772));
#25960=CARTESIAN_POINT('Ctrl Pts',(34.,-32.4,-10.8818602136341));
#25961=CARTESIAN_POINT('Origin',(28.2,-31.9,-4.));
#25962=CARTESIAN_POINT('Origin',(28.2,-32.4,-4.));
#25963=CARTESIAN_POINT('Origin',(28.2,-31.9,-4.));
#25964=CARTESIAN_POINT('',(34.,-31.4,-10.8818602136341));
#25965=CARTESIAN_POINT('',(34.,-31.9,-10.8818602136341));
#25966=CARTESIAN_POINT('',(37.2,-69.5,-4.));
#25967=CARTESIAN_POINT('',(37.2,-31.9,-4.));
#25968=CARTESIAN_POINT('',(28.2,-69.5,-13.));
#25969=CARTESIAN_POINT('Origin',(28.2,-69.5,-4.));
#25970=CARTESIAN_POINT('',(28.2,-31.9,-13.));
#25971=CARTESIAN_POINT('',(28.2,-31.9,-13.));
#25972=CARTESIAN_POINT('',(33.5,-31.9,-11.2739260375673));
#25973=CARTESIAN_POINT('Origin',(28.2,-31.9,-4.));
#25974=CARTESIAN_POINT('Origin',(28.2,-37.2,-4.));
#25975=CARTESIAN_POINT('Origin',(37.2,-31.9,-4.));
#25976=CARTESIAN_POINT('',(37.2,-69.5,4.));
#25977=CARTESIAN_POINT('',(37.2,-31.9,4.));
#25978=CARTESIAN_POINT('',(37.2,-69.5,-2.));
#25979=CARTESIAN_POINT('',(37.2,-61.,1.525));
#25980=CARTESIAN_POINT('Origin',(37.2,-61.,0.));
#25981=CARTESIAN_POINT('Origin',(28.2,-31.9,4.));
#25982=CARTESIAN_POINT('',(34.,-31.4,10.8818602136341));
#25983=CARTESIAN_POINT('',(34.,-31.9,10.8818602136341));
#25984=CARTESIAN_POINT('',(33.5,-31.9,11.2739260375673));
#25985=CARTESIAN_POINT('Origin',(28.2,-37.2,4.));
#25986=CARTESIAN_POINT('',(28.2,-31.9,13.));
#25987=CARTESIAN_POINT('Origin',(28.2,-31.9,4.));
#25988=CARTESIAN_POINT('',(28.2,-69.5,13.));
#25989=CARTESIAN_POINT('',(28.2,-31.9,13.));
#25990=CARTESIAN_POINT('Origin',(28.2,-69.5,4.));
#25991=CARTESIAN_POINT('Origin',(15.2,-0.25,0.));
#25992=CARTESIAN_POINT('',(9.85,0.,6.55186037543834E-16));
#25993=CARTESIAN_POINT('Origin',(15.2,0.,0.));
#25994=CARTESIAN_POINT('',(10.35,-0.5,-5.93953697586466E-16));
#25995=CARTESIAN_POINT('',(10.1,-0.25,6.2456986756515E-16));
#25996=CARTESIAN_POINT('Origin',(15.2,-0.5,0.));
#25997=CARTESIAN_POINT('Origin',(15.2,0.,-2.22044604925031E-15));
#25998=CARTESIAN_POINT('',(33.5,0.,16.8));
#25999=CARTESIAN_POINT('',(32.,0.,18.3));
#26000=CARTESIAN_POINT('Origin',(32.,0.,16.8));
#26001=CARTESIAN_POINT('',(33.5,0.,-16.8));
#26002=CARTESIAN_POINT('',(33.5,0.,-8.4));
#26003=CARTESIAN_POINT('',(32.,0.,-18.3));
#26004=CARTESIAN_POINT('Origin',(32.,0.,-16.8));
#26005=CARTESIAN_POINT('',(-1.6,0.,-18.3));
#26006=CARTESIAN_POINT('',(6.8,0.,-18.3));
#26007=CARTESIAN_POINT('',(-3.1,0.,-16.8));
#26008=CARTESIAN_POINT('Origin',(-1.6,0.,-16.8));
#26009=CARTESIAN_POINT('',(-3.1,0.,16.8));
#26010=CARTESIAN_POINT('',(-3.1,0.,8.4));
#26011=CARTESIAN_POINT('',(-1.6,0.,18.3));
#26012=CARTESIAN_POINT('Origin',(-1.6,0.,16.8));
#26013=CARTESIAN_POINT('',(23.6,0.,18.3));
#26014=CARTESIAN_POINT('Origin',(15.2,0.,0.));
#26015=CARTESIAN_POINT('',(10.35,-32.5,5.93953697586466E-16));
#26016=CARTESIAN_POINT('',(10.35,0.,-5.93953697586466E-16));
#26017=CARTESIAN_POINT('Origin',(15.2,-32.5,0.));
#26018=CARTESIAN_POINT('Origin',(2.2,-32.15,-4.));
#26019=CARTESIAN_POINT('',(-3.6,-31.9,-10.2136945531624));
#26020=CARTESIAN_POINT('',(-3.6,-32.4,-10.8818602136341));
#26021=CARTESIAN_POINT('Ctrl Pts',(-3.6,-32.4,-10.8818602136341));
#26022=CARTESIAN_POINT('Ctrl Pts',(-3.6,-32.1372444185762,-10.5382321596773));
#26023=CARTESIAN_POINT('Ctrl Pts',(-3.6,-31.9,-10.2136945531624));
#26024=CARTESIAN_POINT('',(-6.8,-32.4,-4.));
#26025=CARTESIAN_POINT('Origin',(2.2,-32.4,-4.));
#26026=CARTESIAN_POINT('',(-6.3,-31.9,-4.));
#26027=CARTESIAN_POINT('',(-6.8,-32.4,-4.));
#26028=CARTESIAN_POINT('Origin',(2.2,-31.9,-4.));
#26029=CARTESIAN_POINT('Origin',(-6.55,-32.15,2.));
#26030=CARTESIAN_POINT('',(-6.8,-32.4,4.));
#26031=CARTESIAN_POINT('',(-6.8,-32.4,2.));
#26032=CARTESIAN_POINT('',(-6.3,-31.9,4.));
#26033=CARTESIAN_POINT('',(-6.8,-32.4,4.));
#26034=CARTESIAN_POINT('',(-6.3,-31.9,2.));
#26035=CARTESIAN_POINT('Origin',(2.2,-32.15,4.));
#26036=CARTESIAN_POINT('',(-3.6,-32.4,10.8818602136341));
#26037=CARTESIAN_POINT('',(-3.6,-31.9,10.2136945531624));
#26038=CARTESIAN_POINT('Ctrl Pts',(-3.6,-31.9,10.2136945531624));
#26039=CARTESIAN_POINT('Ctrl Pts',(-3.6,-32.1372444185762,10.5382321596772));
#26040=CARTESIAN_POINT('Ctrl Pts',(-3.6,-32.4,10.8818602136341));
#26041=CARTESIAN_POINT('Origin',(2.2,-31.9,4.));
#26042=CARTESIAN_POINT('Origin',(2.2,-32.4,4.));
#26043=CARTESIAN_POINT('Origin',(2.2,-31.9,4.));
#26044=CARTESIAN_POINT('',(-3.6,-31.4,10.8818602136341));
#26045=CARTESIAN_POINT('',(-3.6,-31.9,10.8818602136341));
#26046=CARTESIAN_POINT('',(-6.8,-69.5,4.));
#26047=CARTESIAN_POINT('',(-6.8,-31.9,4.));
#26048=CARTESIAN_POINT('',(2.2,-69.5,13.));
#26049=CARTESIAN_POINT('Origin',(2.2,-69.5,4.));
#26050=CARTESIAN_POINT('',(2.2,-31.9,13.));
#26051=CARTESIAN_POINT('',(2.2,-31.9,13.));
#26052=CARTESIAN_POINT('',(-3.1,-31.9,11.2739260375673));
#26053=CARTESIAN_POINT('Origin',(2.2,-31.9,4.));
#26054=CARTESIAN_POINT('Origin',(2.2,-37.2,4.));
#26055=CARTESIAN_POINT('Origin',(-6.8,-31.9,4.));
#26056=CARTESIAN_POINT('',(-6.8,-69.5,-4.));
#26057=CARTESIAN_POINT('',(-6.8,-31.9,-4.));
#26058=CARTESIAN_POINT('',(-6.8,-69.5,2.));
#26059=CARTESIAN_POINT('',(-6.8,-61.,1.525));
#26060=CARTESIAN_POINT('Origin',(-6.8,-61.,0.));
#26061=CARTESIAN_POINT('Origin',(2.2,-31.9,-4.));
#26062=CARTESIAN_POINT('',(-3.6,-31.4,-10.8818602136341));
#26063=CARTESIAN_POINT('',(-3.6,-31.9,-10.8818602136341));
#26064=CARTESIAN_POINT('',(-3.1,-31.9,-11.2739260375673));
#26065=CARTESIAN_POINT('Origin',(2.2,-37.2,-4.));
#26066=CARTESIAN_POINT('',(2.2,-31.9,-13.));
#26067=CARTESIAN_POINT('Origin',(2.2,-31.9,-4.));
#26068=CARTESIAN_POINT('',(2.2,-69.5,-13.));
#26069=CARTESIAN_POINT('',(2.2,-31.9,-13.));
#26070=CARTESIAN_POINT('Origin',(2.2,-69.5,-4.));
#26071=CARTESIAN_POINT('Origin',(-3.35,-31.65,8.4));
#26072=CARTESIAN_POINT('',(-3.6,-31.4,-16.8));
#26073=CARTESIAN_POINT('',(-3.6,-31.4,8.4));
#26074=CARTESIAN_POINT('',(-3.1,-31.9,-16.8));
#26075=CARTESIAN_POINT('',(-3.6,-31.4,-16.8));
#26076=CARTESIAN_POINT('',(-3.1,-31.9,8.4));
#26077=CARTESIAN_POINT('Origin',(-1.6,-31.65,-16.8));
#26078=CARTESIAN_POINT('',(-1.6,-31.4,-18.8));
#26079=CARTESIAN_POINT('',(-1.6,-31.9,-18.3));
#26080=CARTESIAN_POINT('',(-1.6,-31.4,-18.8));
#26081=CARTESIAN_POINT('Origin',(-1.6,-31.9,-16.8));
#26082=CARTESIAN_POINT('Origin',(-1.6,-31.4,-16.8));
#26083=CARTESIAN_POINT('Origin',(6.8,-31.65,-18.55));
#26084=CARTESIAN_POINT('',(32.,-31.4,-18.8));
#26085=CARTESIAN_POINT('',(32.,-31.9,-18.3));
#26086=CARTESIAN_POINT('',(32.,-31.4,-18.8));
#26087=CARTESIAN_POINT('',(6.8,-31.9,-18.3));
#26088=CARTESIAN_POINT('',(6.8,-31.4,-18.8));
#26089=CARTESIAN_POINT('Origin',(32.,-31.65,-16.8));
#26090=CARTESIAN_POINT('',(34.,-31.4,-16.8));
#26091=CARTESIAN_POINT('',(33.5,-31.9,-16.8));
#26092=CARTESIAN_POINT('',(34.,-31.4,-16.8));
#26093=CARTESIAN_POINT('Origin',(32.,-31.9,-16.8));
#26094=CARTESIAN_POINT('Origin',(32.,-31.4,-16.8));
#26095=CARTESIAN_POINT('Origin',(33.75,-31.65,-8.4));
#26096=CARTESIAN_POINT('',(33.5,-31.9,-8.4));
#26097=CARTESIAN_POINT('',(34.,-31.4,-8.4));
#26098=CARTESIAN_POINT('Origin',(34.,0.,-16.8));
#26099=CARTESIAN_POINT('',(34.,-0.5,-16.8));
#26100=CARTESIAN_POINT('',(34.,0.,-16.8));
#26101=CARTESIAN_POINT('',(34.,-0.5,16.8));
#26102=CARTESIAN_POINT('',(34.,-0.5,-8.4));
#26103=CARTESIAN_POINT('',(34.,-12.5,16.8));
#26104=CARTESIAN_POINT('',(34.,0.,16.8));
#26105=CARTESIAN_POINT('',(34.,-12.5,15.3));
#26106=CARTESIAN_POINT('',(34.,-12.5,1.));
#26107=CARTESIAN_POINT('',(34.,-19.5,15.3));
#26108=CARTESIAN_POINT('',(34.,-8.,15.3));
#26109=CARTESIAN_POINT('',(34.,-19.5,16.8));
#26110=CARTESIAN_POINT('',(34.,-19.5,1.));
#26111=CARTESIAN_POINT('',(34.,-31.4,16.8));
#26112=CARTESIAN_POINT('',(34.,0.,16.8));
#26113=CARTESIAN_POINT('',(34.,-31.4,-8.4));
#26114=CARTESIAN_POINT('',(34.,-31.9,-16.8));
#26115=CARTESIAN_POINT('Origin',(32.,0.,-16.8));
#26116=CARTESIAN_POINT('',(32.,-0.5,-18.8));
#26117=CARTESIAN_POINT('',(32.,0.,-18.8));
#26118=CARTESIAN_POINT('Origin',(32.,-0.5,-16.8));
#26119=CARTESIAN_POINT('Origin',(-1.6,0.,-18.8));
#26120=CARTESIAN_POINT('',(-1.6,-0.5,-18.8));
#26121=CARTESIAN_POINT('',(-1.6,0.,-18.8));
#26122=CARTESIAN_POINT('',(6.8,-0.5,-18.8));
#26123=CARTESIAN_POINT('Origin',(-1.6,0.,-16.8));
#26124=CARTESIAN_POINT('',(-3.6,-0.5,-16.8));
#26125=CARTESIAN_POINT('',(-3.6,0.,-16.8));
#26126=CARTESIAN_POINT('Origin',(-1.6,-0.5,-16.8));
#26127=CARTESIAN_POINT('Origin',(-3.6,0.,16.8));
#26128=CARTESIAN_POINT('',(-3.6,-31.9,16.8));
#26129=CARTESIAN_POINT('',(-3.6,-31.4,16.8));
#26130=CARTESIAN_POINT('',(-3.6,-31.4,8.4));
#26131=CARTESIAN_POINT('',(-3.6,-19.5,16.8));
#26132=CARTESIAN_POINT('',(-3.6,0.,16.8));
#26133=CARTESIAN_POINT('',(-3.6,-19.5,15.3));
#26134=CARTESIAN_POINT('',(-3.6,-19.5,17.8));
#26135=CARTESIAN_POINT('',(-3.6,-12.5,15.3));
#26136=CARTESIAN_POINT('',(-3.6,-8.,15.3));
#26137=CARTESIAN_POINT('',(-3.6,-12.5,16.8));
#26138=CARTESIAN_POINT('',(-3.6,-12.5,17.8));
#26139=CARTESIAN_POINT('',(-3.6,-0.5,16.8));
#26140=CARTESIAN_POINT('',(-3.6,0.,16.8));
#26141=CARTESIAN_POINT('',(-3.6,-0.5,8.4));
#26142=CARTESIAN_POINT('Origin',(33.75,-31.65,-8.4));
#26143=CARTESIAN_POINT('',(33.5,-31.9,16.8));
#26144=CARTESIAN_POINT('',(34.,-31.4,16.8));
#26145=CARTESIAN_POINT('',(33.5,-31.9,-8.4));
#26146=CARTESIAN_POINT('Origin',(32.,-31.65,16.8));
#26147=CARTESIAN_POINT('',(32.,-31.4,18.8));
#26148=CARTESIAN_POINT('',(32.,-31.9,18.3));
#26149=CARTESIAN_POINT('',(32.,-31.4,18.8));
#26150=CARTESIAN_POINT('Origin',(32.,-31.9,16.8));
#26151=CARTESIAN_POINT('Origin',(32.,-31.4,16.8));
#26152=CARTESIAN_POINT('Origin',(23.6,-31.65,18.55));
#26153=CARTESIAN_POINT('',(-1.6,-31.4,18.8));
#26154=CARTESIAN_POINT('',(-1.6,-31.9,18.3));
#26155=CARTESIAN_POINT('',(-1.6,-31.4,18.8));
#26156=CARTESIAN_POINT('',(23.6,-31.9,18.3));
#26157=CARTESIAN_POINT('',(23.6,-31.4,18.8));
#26158=CARTESIAN_POINT('Origin',(-1.6,-31.65,16.8));
#26159=CARTESIAN_POINT('',(-3.1,-31.9,16.8));
#26160=CARTESIAN_POINT('',(-3.6,-31.4,16.8));
#26161=CARTESIAN_POINT('Origin',(-1.6,-31.9,16.8));
#26162=CARTESIAN_POINT('Origin',(-1.6,-31.4,16.8));
#26163=CARTESIAN_POINT('Origin',(-3.35,-31.65,8.4));
#26164=CARTESIAN_POINT('',(-3.1,-31.9,8.4));
#26165=CARTESIAN_POINT('Origin',(-1.6,0.,16.8));
#26166=CARTESIAN_POINT('',(-1.6,-19.5,18.8));
#26167=CARTESIAN_POINT('',(-1.6,0.,18.8));
#26168=CARTESIAN_POINT('Origin',(-1.6,-19.5,16.8));
#26169=CARTESIAN_POINT('Origin',(32.,0.,18.8));
#26170=CARTESIAN_POINT('',(32.,-19.5,18.8));
#26171=CARTESIAN_POINT('',(32.,0.,18.8));
#26172=CARTESIAN_POINT('',(33.6,-19.5,18.8));
#26173=CARTESIAN_POINT('Origin',(32.,0.,16.8));
#26174=CARTESIAN_POINT('Origin',(32.,-19.5,16.8));
#26175=CARTESIAN_POINT('Origin',(32.,-0.25,16.8));
#26176=CARTESIAN_POINT('',(34.,-0.5,16.8));
#26177=CARTESIAN_POINT('',(32.,-0.5,18.8));
#26178=CARTESIAN_POINT('',(32.,0.,18.3));
#26179=CARTESIAN_POINT('Origin',(32.,-0.5,16.8));
#26180=CARTESIAN_POINT('Origin',(33.75,-0.25,-8.4));
#26181=CARTESIAN_POINT('',(34.,-0.5,-16.8));
#26182=CARTESIAN_POINT('Origin',(32.,-0.25,-16.8));
#26183=CARTESIAN_POINT('',(32.,-0.5,-18.8));
#26184=CARTESIAN_POINT('Origin',(6.8,-0.25,-18.55));
#26185=CARTESIAN_POINT('',(-1.6,-0.5,-18.8));
#26186=CARTESIAN_POINT('Origin',(-1.6,-0.25,-16.8));
#26187=CARTESIAN_POINT('',(-3.6,-0.5,-16.8));
#26188=CARTESIAN_POINT('Origin',(-3.35,-0.25,8.4));
#26189=CARTESIAN_POINT('',(-3.6,-0.5,16.8));
#26190=CARTESIAN_POINT('Origin',(-1.6,-0.25,16.8));
#26191=CARTESIAN_POINT('',(-1.6,-0.5,18.8));
#26192=CARTESIAN_POINT('',(-1.6,-0.5,18.8));
#26193=CARTESIAN_POINT('Origin',(-1.6,-0.5,16.8));
#26194=CARTESIAN_POINT('Origin',(23.6,-0.25,18.55));
#26195=CARTESIAN_POINT('',(23.6,-0.5,18.8));
#26196=CARTESIAN_POINT('Origin',(32.,0.,16.8));
#26197=CARTESIAN_POINT('',(32.,-12.5,18.8));
#26198=CARTESIAN_POINT('',(32.,0.,18.8));
#26199=CARTESIAN_POINT('Origin',(32.,-12.5,16.8));
#26200=CARTESIAN_POINT('Origin',(-3.35,-8.,15.55));
#26201=CARTESIAN_POINT('',(-3.1,-19.,15.8));
#26202=CARTESIAN_POINT('',(-1.10000000000001,-17.,17.8));
#26203=CARTESIAN_POINT('',(-3.1,-13.,15.8));
#26204=CARTESIAN_POINT('',(-3.1,-8.,15.8));
#26205=CARTESIAN_POINT('',(-3.76666666666667,-12.3333333333333,15.1333333333333));
#26206=CARTESIAN_POINT('Origin',(15.2,-16.,15.8));
#26207=CARTESIAN_POINT('',(33.5,-19.,15.8));
#26208=CARTESIAN_POINT('',(-4.8,-19.,15.8));
#26209=CARTESIAN_POINT('',(33.5,-13.,15.8));
#26210=CARTESIAN_POINT('',(33.5,-8.,15.8));
#26211=CARTESIAN_POINT('',(35.2,-13.,15.8));
#26212=CARTESIAN_POINT('Origin',(33.75,-8.,15.55));
#26213=CARTESIAN_POINT('',(36.9666666666667,-9.53333333333332,12.3333333333333));
#26214=CARTESIAN_POINT('',(34.3,-19.8,15.));
#26215=CARTESIAN_POINT('Origin',(28.2,-69.75,-4.));
#26216=CARTESIAN_POINT('',(36.7,-70.,-4.));
#26217=CARTESIAN_POINT('',(37.2,-69.5,-4.));
#26218=CARTESIAN_POINT('',(28.2,-70.,-12.5));
#26219=CARTESIAN_POINT('Origin',(28.2,-70.,-4.));
#26220=CARTESIAN_POINT('',(28.2,-70.,-12.5));
#26221=CARTESIAN_POINT('Origin',(36.95,-69.75,-2.));
#26222=CARTESIAN_POINT('',(36.7,-70.,4.));
#26223=CARTESIAN_POINT('',(37.2,-69.5,4.));
#26224=CARTESIAN_POINT('',(36.7,-70.,-2.));
#26225=CARTESIAN_POINT('Origin',(28.2,-69.75,4.));
#26226=CARTESIAN_POINT('',(28.2,-70.,12.5));
#26227=CARTESIAN_POINT('',(28.2,-69.5,13.));
#26228=CARTESIAN_POINT('Origin',(28.2,-70.,4.));
#26229=CARTESIAN_POINT('Origin',(21.7,-69.75,12.75));
#26230=CARTESIAN_POINT('',(2.2,-70.,12.5));
#26231=CARTESIAN_POINT('',(2.2,-69.5,13.));
#26232=CARTESIAN_POINT('',(21.7,-70.,12.5));
#26233=CARTESIAN_POINT('',(21.7,-69.5,13.));
#26234=CARTESIAN_POINT('Origin',(2.2,-69.75,4.));
#26235=CARTESIAN_POINT('',(-6.3,-70.,4.));
#26236=CARTESIAN_POINT('',(-6.8,-69.5,4.));
#26237=CARTESIAN_POINT('Origin',(2.2,-70.,4.));
#26238=CARTESIAN_POINT('Origin',(-6.55,-69.75,2.));
#26239=CARTESIAN_POINT('',(-6.3,-70.,-4.));
#26240=CARTESIAN_POINT('',(-6.8,-69.5,-4.));
#26241=CARTESIAN_POINT('',(-6.3,-70.,2.));
#26242=CARTESIAN_POINT('Origin',(2.2,-69.75,-4.));
#26243=CARTESIAN_POINT('',(2.2,-70.,-12.5));
#26244=CARTESIAN_POINT('',(2.2,-69.5,-13.));
#26245=CARTESIAN_POINT('Origin',(2.2,-70.,-4.));
#26246=CARTESIAN_POINT('Origin',(8.7,-69.75,-12.75));
#26247=CARTESIAN_POINT('',(8.7,-70.,-12.5));
#26248=CARTESIAN_POINT('',(8.7,-69.5,-13.));
#26249=CARTESIAN_POINT('Origin',(28.2,-31.9,13.));
#26250=CARTESIAN_POINT('',(21.7,-31.9,13.));
#26251=CARTESIAN_POINT('Origin',(15.2,-70.,0.));
#26252=CARTESIAN_POINT('',(26.,-70.,9.8));
#26253=CARTESIAN_POINT('',(26.,-70.,-9.8));
#26254=CARTESIAN_POINT('',(26.,-70.,-4.65));
#26255=CARTESIAN_POINT('',(34.4,-70.,9.8));
#26256=CARTESIAN_POINT('',(20.85,-70.,9.8));
#26257=CARTESIAN_POINT('',(34.4,-70.,-9.8));
#26258=CARTESIAN_POINT('',(34.4,-70.,4.65));
#26259=CARTESIAN_POINT('',(24.55,-70.,-9.8));
#26260=CARTESIAN_POINT('',(6.,-70.,9.8));
#26261=CARTESIAN_POINT('',(6.,-70.,-9.8));
#26262=CARTESIAN_POINT('',(6.,-70.,-4.65));
#26263=CARTESIAN_POINT('',(14.4,-70.,9.8));
#26264=CARTESIAN_POINT('',(10.85,-70.,9.8));
#26265=CARTESIAN_POINT('',(14.4,-70.,-9.8));
#26266=CARTESIAN_POINT('',(14.4,-70.,4.65));
#26267=CARTESIAN_POINT('',(14.55,-70.,-9.8));
#26268=CARTESIAN_POINT('',(16.,-70.,9.8));
#26269=CARTESIAN_POINT('',(16.,-70.,-9.8));
#26270=CARTESIAN_POINT('',(16.,-70.,-4.65));
#26271=CARTESIAN_POINT('',(24.4,-70.,9.8));
#26272=CARTESIAN_POINT('',(15.85,-70.,9.8));
#26273=CARTESIAN_POINT('',(24.4,-70.,-9.8));
#26274=CARTESIAN_POINT('',(24.4,-70.,4.65));
#26275=CARTESIAN_POINT('',(19.55,-70.,-9.8));
#26276=CARTESIAN_POINT('',(-4.,-70.,9.8));
#26277=CARTESIAN_POINT('',(-4.,-70.,-9.8));
#26278=CARTESIAN_POINT('',(-4.,-70.,-4.65));
#26279=CARTESIAN_POINT('',(4.4,-70.,9.8));
#26280=CARTESIAN_POINT('',(5.85,-70.,9.8));
#26281=CARTESIAN_POINT('',(4.4,-70.,-9.8));
#26282=CARTESIAN_POINT('',(4.4,-70.,4.65));
#26283=CARTESIAN_POINT('',(9.55,-70.,-9.8));
#26284=CARTESIAN_POINT('Origin',(-3.35,-12.75,17.8));
#26285=CARTESIAN_POINT('',(-3.1,-13.,16.8));
#26286=CARTESIAN_POINT('',(-3.1,-13.,17.8));
#26287=CARTESIAN_POINT('',(-3.1,-13.,16.8));
#26288=CARTESIAN_POINT('Origin',(-1.6,-12.75,16.8));
#26289=CARTESIAN_POINT('',(-1.6,-13.,18.3));
#26290=CARTESIAN_POINT('',(-1.6,-12.5,18.8));
#26291=CARTESIAN_POINT('',(-1.6,-13.,18.3));
#26292=CARTESIAN_POINT('Origin',(-1.6,-12.5,16.8));
#26293=CARTESIAN_POINT('Origin',(-1.6,-13.,16.8));
#26294=CARTESIAN_POINT('Origin',(13.6,-12.75,18.55));
#26295=CARTESIAN_POINT('',(32.,-13.,18.3));
#26296=CARTESIAN_POINT('',(32.,-13.,18.3));
#26297=CARTESIAN_POINT('',(13.6,-12.5,18.8));
#26298=CARTESIAN_POINT('',(13.6,-13.,18.3));
#26299=CARTESIAN_POINT('Origin',(32.,-12.75,16.8));
#26300=CARTESIAN_POINT('',(33.5,-13.,16.8));
#26301=CARTESIAN_POINT('',(33.5,-13.,16.8));
#26302=CARTESIAN_POINT('Origin',(32.,-13.,16.8));
#26303=CARTESIAN_POINT('Origin',(33.75,-12.75,1.));
#26304=CARTESIAN_POINT('',(33.5,-13.,1.));
#26305=CARTESIAN_POINT('Origin',(-4.8,-13.,18.8));
#26306=CARTESIAN_POINT('Origin',(33.75,-19.25,1.));
#26307=CARTESIAN_POINT('',(33.5,-19.,16.8));
#26308=CARTESIAN_POINT('',(33.5,-19.,1.));
#26309=CARTESIAN_POINT('',(33.5,-19.,16.8));
#26310=CARTESIAN_POINT('Origin',(32.,-19.25,16.8));
#26311=CARTESIAN_POINT('',(32.,-19.,18.3));
#26312=CARTESIAN_POINT('',(32.,-19.,18.3));
#26313=CARTESIAN_POINT('Origin',(32.,-19.,16.8));
#26314=CARTESIAN_POINT('Origin',(33.6,-19.25,18.55));
#26315=CARTESIAN_POINT('',(-1.6,-19.,18.3));
#26316=CARTESIAN_POINT('',(-1.6,-19.,18.3));
#26317=CARTESIAN_POINT('',(33.6,-19.,18.3));
#26318=CARTESIAN_POINT('Origin',(-1.6,-19.25,16.8));
#26319=CARTESIAN_POINT('',(-3.1,-19.,16.8));
#26320=CARTESIAN_POINT('',(-3.1,-19.,16.8));
#26321=CARTESIAN_POINT('Origin',(-1.6,-19.,16.8));
#26322=CARTESIAN_POINT('Origin',(-3.35,-19.25,17.8));
#26323=CARTESIAN_POINT('',(-3.1,-19.,17.8));
#26324=CARTESIAN_POINT('Origin',(35.2,-19.,18.8));
#26325=CARTESIAN_POINT('Origin',(34.15,-69.75,4.65));
#26326=CARTESIAN_POINT('',(33.9,-69.5,9.3));
#26327=CARTESIAN_POINT('',(34.4,-70.,9.8));
#26328=CARTESIAN_POINT('',(33.9,-69.5,-9.3));
#26329=CARTESIAN_POINT('',(33.9,-69.5,4.65));
#26330=CARTESIAN_POINT('',(34.4,-70.,-9.8));
#26331=CARTESIAN_POINT('Origin',(26.25,-69.75,-4.65));
#26332=CARTESIAN_POINT('',(26.5,-69.5,-9.3));
#26333=CARTESIAN_POINT('',(26.,-70.,-9.8));
#26334=CARTESIAN_POINT('',(26.5,-69.5,9.3));
#26335=CARTESIAN_POINT('',(26.5,-69.5,-4.65));
#26336=CARTESIAN_POINT('',(26.5,-69.5,9.3));
#26337=CARTESIAN_POINT('Origin',(24.55,-69.75,-9.55));
#26338=CARTESIAN_POINT('',(24.55,-69.5,-9.3));
#26339=CARTESIAN_POINT('Origin',(20.85,-69.75,9.55));
#26340=CARTESIAN_POINT('',(20.85,-69.5,9.3));
#26341=CARTESIAN_POINT('Origin',(26.5,-70.,9.3));
#26342=CARTESIAN_POINT('',(26.5,-52.,9.3));
#26343=CARTESIAN_POINT('',(26.5,-70.,9.3));
#26344=CARTESIAN_POINT('',(33.9,-52.,9.3));
#26345=CARTESIAN_POINT('',(33.9,-52.,9.3));
#26346=CARTESIAN_POINT('',(33.9,-70.,9.3));
#26347=CARTESIAN_POINT('Origin',(26.5,-70.,-9.3));
#26348=CARTESIAN_POINT('',(26.5,-52.,-9.3));
#26349=CARTESIAN_POINT('',(26.5,-70.,-9.3));
#26350=CARTESIAN_POINT('',(26.5,-52.,9.3));
#26351=CARTESIAN_POINT('',(26.5,-61.,1.525));
#26352=CARTESIAN_POINT('Origin',(26.5,-61.,0.));
#26353=CARTESIAN_POINT('Origin',(4.15,-69.75,4.65));
#26354=CARTESIAN_POINT('',(3.9,-69.5,9.3));
#26355=CARTESIAN_POINT('',(4.4,-70.,9.8));
#26356=CARTESIAN_POINT('',(3.9,-69.5,-9.3));
#26357=CARTESIAN_POINT('',(3.9,-69.5,4.65));
#26358=CARTESIAN_POINT('',(4.4,-70.,-9.8));
#26359=CARTESIAN_POINT('Origin',(-3.75,-69.75,-4.65));
#26360=CARTESIAN_POINT('',(-3.5,-69.5,-9.3));
#26361=CARTESIAN_POINT('',(-4.,-70.,-9.8));
#26362=CARTESIAN_POINT('',(-3.5,-69.5,9.3));
#26363=CARTESIAN_POINT('',(-3.5,-69.5,-4.65));
#26364=CARTESIAN_POINT('',(-3.5,-69.5,9.3));
#26365=CARTESIAN_POINT('Origin',(9.55,-69.75,-9.55));
#26366=CARTESIAN_POINT('',(9.55,-69.5,-9.3));
#26367=CARTESIAN_POINT('Origin',(5.85,-69.75,9.55));
#26368=CARTESIAN_POINT('',(5.85,-69.5,9.3));
#26369=CARTESIAN_POINT('Origin',(-3.5,-70.,9.3));
#26370=CARTESIAN_POINT('',(-3.5,-52.,9.3));
#26371=CARTESIAN_POINT('',(-3.5,-70.,9.3));
#26372=CARTESIAN_POINT('',(3.9,-52.,9.3));
#26373=CARTESIAN_POINT('',(3.9,-52.,9.3));
#26374=CARTESIAN_POINT('',(3.9,-70.,9.3));
#26375=CARTESIAN_POINT('Origin',(-3.5,-70.,-9.3));
#26376=CARTESIAN_POINT('',(-3.5,-52.,-9.3));
#26377=CARTESIAN_POINT('',(-3.5,-70.,-9.3));
#26378=CARTESIAN_POINT('',(-3.5,-52.,9.3));
#26379=CARTESIAN_POINT('',(-3.5,-61.,1.525));
#26380=CARTESIAN_POINT('Origin',(-3.5,-61.,0.));
#26381=CARTESIAN_POINT('Origin',(14.15,-69.75,4.65));
#26382=CARTESIAN_POINT('',(13.9,-69.5,9.3));
#26383=CARTESIAN_POINT('',(14.4,-70.,9.8));
#26384=CARTESIAN_POINT('',(13.9,-69.5,-9.3));
#26385=CARTESIAN_POINT('',(13.9,-69.5,4.65));
#26386=CARTESIAN_POINT('',(14.4,-70.,-9.8));
#26387=CARTESIAN_POINT('Origin',(6.25,-69.75,-4.65));
#26388=CARTESIAN_POINT('',(6.5,-69.5,-9.3));
#26389=CARTESIAN_POINT('',(6.,-70.,-9.8));
#26390=CARTESIAN_POINT('',(6.5,-69.5,9.3));
#26391=CARTESIAN_POINT('',(6.5,-69.5,-4.65));
#26392=CARTESIAN_POINT('',(6.5,-69.5,9.3));
#26393=CARTESIAN_POINT('Origin',(14.55,-69.75,-9.55));
#26394=CARTESIAN_POINT('',(14.55,-69.5,-9.3));
#26395=CARTESIAN_POINT('Origin',(10.85,-69.75,9.55));
#26396=CARTESIAN_POINT('',(10.85,-69.5,9.3));
#26397=CARTESIAN_POINT('Origin',(6.5,-70.,9.3));
#26398=CARTESIAN_POINT('',(6.5,-52.,9.3));
#26399=CARTESIAN_POINT('',(6.5,-70.,9.3));
#26400=CARTESIAN_POINT('',(13.9,-52.,9.3));
#26401=CARTESIAN_POINT('',(13.9,-52.,9.3));
#26402=CARTESIAN_POINT('',(13.9,-70.,9.3));
#26403=CARTESIAN_POINT('Origin',(6.5,-70.,-9.3));
#26404=CARTESIAN_POINT('',(6.5,-52.,-9.3));
#26405=CARTESIAN_POINT('',(6.5,-70.,-9.3));
#26406=CARTESIAN_POINT('',(6.5,-52.,9.3));
#26407=CARTESIAN_POINT('',(6.5,-61.,1.525));
#26408=CARTESIAN_POINT('Origin',(6.5,-61.,0.));
#26409=CARTESIAN_POINT('Origin',(24.15,-69.75,4.65));
#26410=CARTESIAN_POINT('',(23.9,-69.5,9.3));
#26411=CARTESIAN_POINT('',(24.4,-70.,9.8));
#26412=CARTESIAN_POINT('',(23.9,-69.5,-9.3));
#26413=CARTESIAN_POINT('',(23.9,-69.5,4.65));
#26414=CARTESIAN_POINT('',(24.4,-70.,-9.8));
#26415=CARTESIAN_POINT('Origin',(16.25,-69.75,-4.65));
#26416=CARTESIAN_POINT('',(16.5,-69.5,-9.3));
#26417=CARTESIAN_POINT('',(16.,-70.,-9.8));
#26418=CARTESIAN_POINT('',(16.5,-69.5,9.3));
#26419=CARTESIAN_POINT('',(16.5,-69.5,-4.65));
#26420=CARTESIAN_POINT('',(16.5,-69.5,9.3));
#26421=CARTESIAN_POINT('Origin',(19.55,-69.75,-9.55));
#26422=CARTESIAN_POINT('',(19.55,-69.5,-9.3));
#26423=CARTESIAN_POINT('Origin',(15.85,-69.75,9.55));
#26424=CARTESIAN_POINT('',(15.85,-69.5,9.3));
#26425=CARTESIAN_POINT('Origin',(16.5,-70.,9.3));
#26426=CARTESIAN_POINT('',(16.5,-52.,9.3));
#26427=CARTESIAN_POINT('',(16.5,-70.,9.3));
#26428=CARTESIAN_POINT('',(23.9,-52.,9.3));
#26429=CARTESIAN_POINT('',(23.9,-52.,9.3));
#26430=CARTESIAN_POINT('',(23.9,-70.,9.3));
#26431=CARTESIAN_POINT('Origin',(16.5,-70.,-9.3));
#26432=CARTESIAN_POINT('',(16.5,-52.,-9.3));
#26433=CARTESIAN_POINT('',(16.5,-70.,-9.3));
#26434=CARTESIAN_POINT('',(16.5,-52.,9.3));
#26435=CARTESIAN_POINT('',(16.5,-61.,1.525));
#26436=CARTESIAN_POINT('Origin',(16.5,-61.,0.));
#26437=CARTESIAN_POINT('Origin',(37.3,-61.,0.));
#26438=CARTESIAN_POINT('',(33.9,-61.,1.525));
#26439=CARTESIAN_POINT('',(37.3,-61.,1.525));
#26440=CARTESIAN_POINT('Origin',(33.9,-61.,0.));
#26441=CARTESIAN_POINT('Origin',(37.3,-61.,0.));
#26442=CARTESIAN_POINT('',(3.9,-61.,1.525));
#26443=CARTESIAN_POINT('',(37.3,-61.,1.525));
#26444=CARTESIAN_POINT('Origin',(3.9,-61.,0.));
#26445=CARTESIAN_POINT('Origin',(37.3,-61.,0.));
#26446=CARTESIAN_POINT('',(13.9,-61.,1.525));
#26447=CARTESIAN_POINT('',(37.3,-61.,1.525));
#26448=CARTESIAN_POINT('Origin',(13.9,-61.,0.));
#26449=CARTESIAN_POINT('Origin',(37.3,-61.,0.));
#26450=CARTESIAN_POINT('',(23.9,-61.,1.525));
#26451=CARTESIAN_POINT('',(37.3,-61.,1.525));
#26452=CARTESIAN_POINT('Origin',(23.9,-61.,0.));
#26453=CARTESIAN_POINT('Origin',(37.3,-61.,0.));
#26454=CARTESIAN_POINT('',(37.3,-61.,1.525));
#26455=CARTESIAN_POINT('Origin',(23.9,-70.,-9.3));
#26456=CARTESIAN_POINT('',(23.9,-52.,-9.3));
#26457=CARTESIAN_POINT('',(23.9,-70.,-9.3));
#26458=CARTESIAN_POINT('',(16.5,-52.,-9.3));
#26459=CARTESIAN_POINT('Origin',(23.9,-70.,9.3));
#26460=CARTESIAN_POINT('',(23.9,-52.,-9.3));
#26461=CARTESIAN_POINT('Origin',(20.2,-52.,0.));
#26462=CARTESIAN_POINT('Origin',(13.9,-70.,-9.3));
#26463=CARTESIAN_POINT('',(13.9,-52.,-9.3));
#26464=CARTESIAN_POINT('',(13.9,-70.,-9.3));
#26465=CARTESIAN_POINT('',(6.5,-52.,-9.3));
#26466=CARTESIAN_POINT('Origin',(13.9,-70.,9.3));
#26467=CARTESIAN_POINT('',(13.9,-52.,-9.3));
#26468=CARTESIAN_POINT('Origin',(10.2,-52.,0.));
#26469=CARTESIAN_POINT('Origin',(3.9,-70.,-9.3));
#26470=CARTESIAN_POINT('',(3.9,-52.,-9.3));
#26471=CARTESIAN_POINT('',(3.9,-70.,-9.3));
#26472=CARTESIAN_POINT('',(-3.5,-52.,-9.3));
#26473=CARTESIAN_POINT('Origin',(3.9,-70.,9.3));
#26474=CARTESIAN_POINT('',(3.9,-52.,-9.3));
#26475=CARTESIAN_POINT('Origin',(0.199999999999999,-52.,0.));
#26476=CARTESIAN_POINT('Origin',(33.9,-70.,-9.3));
#26477=CARTESIAN_POINT('',(33.9,-52.,-9.3));
#26478=CARTESIAN_POINT('',(33.9,-70.,-9.3));
#26479=CARTESIAN_POINT('',(26.5,-52.,-9.3));
#26480=CARTESIAN_POINT('Origin',(33.9,-70.,9.3));
#26481=CARTESIAN_POINT('',(33.9,-52.,-9.3));
#26482=CARTESIAN_POINT('Origin',(30.2,-52.,0.));
#26483=CARTESIAN_POINT('Origin',(32.,0.,18.8));
#26484=CARTESIAN_POINT('',(-1.6,0.,18.8));
#26485=CARTESIAN_POINT('Origin',(-1.6,0.,16.8));
#26486=CARTESIAN_POINT('Origin',(15.2,-32.5,0.));
#26487=CARTESIAN_POINT('Origin',(15.2,-31.9,0.));
#26488=CARTESIAN_POINT('Origin',(15.2,-31.9,0.));
#26489=CARTESIAN_POINT('Origin',(2.2,-31.9,-13.));
#26490=CARTESIAN_POINT('',(8.7,-31.9,-13.));
#26491=CARTESIAN_POINT('Origin',(15.2,-31.9,-2.22044604925031E-15));
#26492=CARTESIAN_POINT('Origin',(15.2,-31.9,-2.22044604925031E-15));
#26493=CARTESIAN_POINT('',(0.,0.,0.));
#26494=CARTESIAN_POINT('Origin',(30.2656497115746,0.,-1.29160453950038E-16));
#26495=CARTESIAN_POINT('',(30.4,3.57,-4.37198907295605E-16));
#26496=CARTESIAN_POINT('Origin',(30.4,0.,0.));
#26497=CARTESIAN_POINT('',(30.1312994231491,4.21870057685089,5.16641815800153E-16));
#26498=CARTESIAN_POINT('',(30.2656497115746,3.89435028842544,4.76920361547879E-16));
#26499=CARTESIAN_POINT('',(30.1312994231491,-4.21870057685089,-5.16641815800153E-16));
#26500=CARTESIAN_POINT('Origin',(30.1312994231491,0.,-2.58320907900077E-16));
#26501=CARTESIAN_POINT('Origin',(30.1312994231491,0.,-2.58320907900077E-16));
#26502=CARTESIAN_POINT('Origin',(30.,0.,0.));
#26503=CARTESIAN_POINT('',(29.8687005768509,-4.48129942314911,-5.48800899458044E-16));
#26504=CARTESIAN_POINT('',(30.,-4.35,-5.32721357629099E-16));
#26505=CARTESIAN_POINT('',(29.8687005768509,4.48129942314911,-5.48800899458044E-16));
#26506=CARTESIAN_POINT('Origin',(29.8687005768509,0.,-2.74400449729022E-16));
#26507=CARTESIAN_POINT('Origin',(29.8687005768509,0.,-2.74400449729022E-16));
#26508=CARTESIAN_POINT('Origin',(30.4,0.,0.));
#26509=CARTESIAN_POINT('Origin',(29.5443502884254,0.,-1.37200224864511E-16));
#26510=CARTESIAN_POINT('',(29.22,4.75,5.81707229594993E-16));
#26511=CARTESIAN_POINT('',(29.5443502884254,4.61564971157455,5.65254064526518E-16));
#26512=CARTESIAN_POINT('',(29.22,-4.75,-5.81707229594993E-16));
#26513=CARTESIAN_POINT('Origin',(29.22,0.,0.));
#26514=CARTESIAN_POINT('Origin',(29.22,0.,0.));
#26515=CARTESIAN_POINT('Origin',(15.,0.,0.));
#26516=CARTESIAN_POINT('',(0.4,-4.75,-5.81707229594993E-16));
#26517=CARTESIAN_POINT('',(15.,-4.75,-5.81707229594993E-16));
#26518=CARTESIAN_POINT('Origin',(0.4,0.,0.));
#26519=CARTESIAN_POINT('Origin',(0.,4.25,0.));
#26520=CARTESIAN_POINT('',(1.04083408558608E-16,-4.25,-5.20474889637625E-16));
#26521=CARTESIAN_POINT('Origin',(0.,0.,0.));
#26522=CARTESIAN_POINT('Origin',(0.2,0.,0.));
#26523=CARTESIAN_POINT('',(0.2,-4.5,-5.51091059616309E-16));
#26524=CARTESIAN_POINT('',(0.,0.,0.));
#26525=CARTESIAN_POINT('Origin',(0.,1.2,0.));
#26526=CARTESIAN_POINT('',(5.3776427755281E-16,-1.2,-1.46957615897682E-16));
#26527=CARTESIAN_POINT('Origin',(0.,0.,0.));
#26528=CARTESIAN_POINT('Origin',(0.150000000000001,0.,0.));
#26529=CARTESIAN_POINT('',(0.3,-1.5,-1.83697019872103E-16));
#26530=CARTESIAN_POINT('Origin',(0.299999999999998,0.,0.));
#26531=CARTESIAN_POINT('',(0.150000000000001,-1.35,-1.65327317884893E-16));
#26532=CARTESIAN_POINT('Origin',(19.5,0.,0.));
#26533=CARTESIAN_POINT('',(38.7,-1.5,-1.83697019872103E-16));
#26534=CARTESIAN_POINT('Origin',(38.7,0.,0.));
#26535=CARTESIAN_POINT('',(19.5,-1.5,-1.83697019872103E-16));
#26536=CARTESIAN_POINT('Origin',(38.85,0.,0.));
#26537=CARTESIAN_POINT('',(39.,-1.2,-1.46957615897682E-16));
#26538=CARTESIAN_POINT('Origin',(39.,0.,0.));
#26539=CARTESIAN_POINT('',(38.85,-1.35,-1.65327317884893E-16));
#26540=CARTESIAN_POINT('Origin',(39.,0.,0.));
#26541=CARTESIAN_POINT('',(0.,0.,0.));
#26542=CARTESIAN_POINT('Origin',(0.,1.57407089715261,0.831084117726459));
#26543=CARTESIAN_POINT('',(0.,1.57407089715261,0.831084117726459));
#26544=CARTESIAN_POINT('',(0.,1.72712639277127,0.430620974167409));
#26545=CARTESIAN_POINT('',(0.,1.57407089715261,0.831084117726459));
#26546=CARTESIAN_POINT('',(12.,1.72712639277127,0.430620974167409));
#26547=CARTESIAN_POINT('',(0.,1.72712639277127,0.430620974167409));
#26548=CARTESIAN_POINT('',(12.,1.57407089715261,0.831084117726459));
#26549=CARTESIAN_POINT('',(12.,1.57407089715261,0.831084117726459));
#26550=CARTESIAN_POINT('',(0.,1.57407089715261,0.831084117726459));
#26551=CARTESIAN_POINT('Origin',(0.,1.32970462680897,1.18333664079281));
#26552=CARTESIAN_POINT('',(0.,1.32970462680897,1.18333664079281));
#26553=CARTESIAN_POINT('',(0.,1.32970462680897,1.18333664079281));
#26554=CARTESIAN_POINT('',(12.,1.32970462680897,1.18333664079281));
#26555=CARTESIAN_POINT('',(12.,1.32970462680897,1.18333664079281));
#26556=CARTESIAN_POINT('',(0.,1.32970462680897,1.18333664079281));
#26557=CARTESIAN_POINT('Origin',(0.,1.0082031017262,1.46694461574719));
#26558=CARTESIAN_POINT('',(0.,1.0082031017262,1.46694461574719));
#26559=CARTESIAN_POINT('',(0.,1.0082031017262,1.46694461574719));
#26560=CARTESIAN_POINT('',(12.,1.0082031017262,1.46694461574719));
#26561=CARTESIAN_POINT('',(12.,1.0082031017262,1.46694461574719));
#26562=CARTESIAN_POINT('',(0.,1.0082031017262,1.46694461574719));
#26563=CARTESIAN_POINT('Origin',(0.,0.628216405190687,1.66545613819437));
#26564=CARTESIAN_POINT('',(0.,0.628216405190687,1.66545613819437));
#26565=CARTESIAN_POINT('',(0.,0.628216405190687,1.66545613819437));
#26566=CARTESIAN_POINT('',(12.,0.628216405190687,1.66545613819437));
#26567=CARTESIAN_POINT('',(12.,0.628216405190687,1.66545613819437));
#26568=CARTESIAN_POINT('',(0.,0.628216405190687,1.66545613819437));
#26569=CARTESIAN_POINT('Origin',(0.,0.211787305230605,1.76735569066987));
#26570=CARTESIAN_POINT('',(0.,0.211787305230605,1.76735569066987));
#26571=CARTESIAN_POINT('',(0.,0.211787305230605,1.76735569066987));
#26572=CARTESIAN_POINT('',(12.,0.211787305230605,1.76735569066987));
#26573=CARTESIAN_POINT('',(12.,0.211787305230605,1.76735569066987));
#26574=CARTESIAN_POINT('',(0.,0.211787305230605,1.76735569066987));
#26575=CARTESIAN_POINT('Origin',(0.,-0.216927431261162,1.76673214992155));
#26576=CARTESIAN_POINT('',(0.,-0.216927431261162,1.76673214992155));
#26577=CARTESIAN_POINT('',(0.,-0.216927431261162,1.76673214992155));
#26578=CARTESIAN_POINT('',(12.,-0.216927431261162,1.76673214992155));
#26579=CARTESIAN_POINT('',(12.,-0.216927431261162,1.76673214992155));
#26580=CARTESIAN_POINT('',(0.,-0.216927431261162,1.76673214992155));
#26581=CARTESIAN_POINT('Origin',(0.,-0.63305835603048,1.6636216871212));
#26582=CARTESIAN_POINT('',(0.,-0.63305835603048,1.6636216871212));
#26583=CARTESIAN_POINT('',(0.,-0.63305835603048,1.6636216871212));
#26584=CARTESIAN_POINT('',(12.,-0.63305835603048,1.6636216871212));
#26585=CARTESIAN_POINT('',(12.,-0.63305835603048,1.6636216871212));
#26586=CARTESIAN_POINT('',(0.,-0.63305835603048,1.6636216871212));
#26587=CARTESIAN_POINT('Origin',(0.,-1.01246599912308,1.46400566959958));
#26588=CARTESIAN_POINT('',(0.,-1.01246599912308,1.46400566959958));
#26589=CARTESIAN_POINT('',(0.,-1.01246599912308,1.46400566959958));
#26590=CARTESIAN_POINT('',(12.,-1.01246599912308,1.46400566959958));
#26591=CARTESIAN_POINT('',(12.,-1.01246599912308,1.46400566959958));
#26592=CARTESIAN_POINT('',(0.,-1.01246599912308,1.46400566959958));
#26593=CARTESIAN_POINT('Origin',(0.,-1.33314118300442,1.17946368582401));
#26594=CARTESIAN_POINT('',(0.,-1.33314118300442,1.17946368582401));
#26595=CARTESIAN_POINT('',(0.,-1.33314118300442,1.17946368582401));
#26596=CARTESIAN_POINT('',(12.,-1.33314118300442,1.17946368582401));
#26597=CARTESIAN_POINT('',(12.,-1.33314118300442,1.17946368582401));
#26598=CARTESIAN_POINT('',(0.,-1.33314118300442,1.17946368582401));
#26599=CARTESIAN_POINT('Origin',(0.,-1.5764817598753,0.826501821401781));
#26600=CARTESIAN_POINT('',(0.,-1.5764817598753,0.826501821401781));
#26601=CARTESIAN_POINT('',(0.,-1.5764817598753,0.826501821401781));
#26602=CARTESIAN_POINT('',(12.,-1.57648175987531,0.826501821401781));
#26603=CARTESIAN_POINT('',(12.,-1.5764817598753,0.826501821401781));
#26604=CARTESIAN_POINT('',(0.,-1.5764817598753,0.826501821401781));
#26605=CARTESIAN_POINT('Origin',(0.,-1.72837170952577,0.425595152358411));
#26606=CARTESIAN_POINT('',(0.,-1.72837170952577,0.425595152358411));
#26607=CARTESIAN_POINT('',(0.,-1.72837170952577,0.425595152358411));
#26608=CARTESIAN_POINT('',(12.,-1.72837170952577,0.425595152358411));
#26609=CARTESIAN_POINT('',(12.,-1.72837170952577,0.425595152358411));
#26610=CARTESIAN_POINT('',(0.,-1.72837170952577,0.425595152358411));
#26611=CARTESIAN_POINT('Origin',(0.,-1.78,1.00846592378134E-15));
#26612=CARTESIAN_POINT('',(0.,-1.78,1.00846592378134E-15));
#26613=CARTESIAN_POINT('',(0.,-1.78,1.00846592378134E-15));
#26614=CARTESIAN_POINT('',(12.,-1.78,1.04083408558608E-15));
#26615=CARTESIAN_POINT('',(12.,-1.78,1.00846592378134E-15));
#26616=CARTESIAN_POINT('',(0.,-1.78,1.00846592378134E-15));
#26617=CARTESIAN_POINT('Origin',(0.,-1.72837170952577,-0.42559515235841));
#26618=CARTESIAN_POINT('',(0.,-1.72837170952577,-0.42559515235841));
#26619=CARTESIAN_POINT('',(0.,-1.72837170952577,-0.42559515235841));
#26620=CARTESIAN_POINT('',(12.,-1.72837170952577,-0.42559515235841));
#26621=CARTESIAN_POINT('',(12.,-1.72837170952577,-0.42559515235841));
#26622=CARTESIAN_POINT('',(0.,-1.72837170952577,-0.42559515235841));
#26623=CARTESIAN_POINT('Origin',(0.,-1.57648175987531,-0.826501821401781));
#26624=CARTESIAN_POINT('',(0.,-1.57648175987531,-0.826501821401781));
#26625=CARTESIAN_POINT('',(0.,-1.57648175987531,-0.826501821401781));
#26626=CARTESIAN_POINT('',(12.,-1.57648175987531,-0.826501821401781));
#26627=CARTESIAN_POINT('',(12.,-1.57648175987531,-0.826501821401781));
#26628=CARTESIAN_POINT('',(0.,-1.57648175987531,-0.826501821401781));
#26629=CARTESIAN_POINT('Origin',(0.,-1.33314118300442,-1.17946368582401));
#26630=CARTESIAN_POINT('',(0.,-1.33314118300442,-1.17946368582401));
#26631=CARTESIAN_POINT('',(0.,-1.33314118300442,-1.17946368582401));
#26632=CARTESIAN_POINT('',(12.,-1.33314118300442,-1.17946368582401));
#26633=CARTESIAN_POINT('',(12.,-1.33314118300442,-1.17946368582401));
#26634=CARTESIAN_POINT('',(0.,-1.33314118300442,-1.17946368582401));
#26635=CARTESIAN_POINT('Origin',(0.,-1.01246599912308,-1.46400566959958));
#26636=CARTESIAN_POINT('',(0.,-1.01246599912308,-1.46400566959958));
#26637=CARTESIAN_POINT('',(0.,-1.01246599912308,-1.46400566959958));
#26638=CARTESIAN_POINT('',(12.,-1.01246599912308,-1.46400566959958));
#26639=CARTESIAN_POINT('',(12.,-1.01246599912308,-1.46400566959958));
#26640=CARTESIAN_POINT('',(0.,-1.01246599912308,-1.46400566959958));
#26641=CARTESIAN_POINT('Origin',(0.,-0.63305835603048,-1.6636216871212));
#26642=CARTESIAN_POINT('',(0.,-0.63305835603048,-1.6636216871212));
#26643=CARTESIAN_POINT('',(0.,-0.63305835603048,-1.6636216871212));
#26644=CARTESIAN_POINT('',(12.,-0.63305835603048,-1.6636216871212));
#26645=CARTESIAN_POINT('',(12.,-0.63305835603048,-1.6636216871212));
#26646=CARTESIAN_POINT('',(0.,-0.63305835603048,-1.6636216871212));
#26647=CARTESIAN_POINT('Origin',(0.,-0.216927431261162,-1.76673214992155));
#26648=CARTESIAN_POINT('',(0.,-0.216927431261162,-1.76673214992155));
#26649=CARTESIAN_POINT('',(0.,-0.216927431261162,-1.76673214992155));
#26650=CARTESIAN_POINT('',(12.,-0.216927431261162,-1.76673214992155));
#26651=CARTESIAN_POINT('',(12.,-0.216927431261162,-1.76673214992155));
#26652=CARTESIAN_POINT('',(0.,-0.216927431261162,-1.76673214992155));
#26653=CARTESIAN_POINT('Origin',(0.,0.211787305230605,-1.76735569066987));
#26654=CARTESIAN_POINT('',(0.,0.211787305230605,-1.76735569066987));
#26655=CARTESIAN_POINT('',(0.,0.211787305230605,-1.76735569066987));
#26656=CARTESIAN_POINT('',(12.,0.211787305230605,-1.76735569066987));
#26657=CARTESIAN_POINT('',(12.,0.211787305230605,-1.76735569066987));
#26658=CARTESIAN_POINT('',(0.,0.211787305230605,-1.76735569066987));
#26659=CARTESIAN_POINT('Origin',(0.,0.628216405190687,-1.66545613819437));
#26660=CARTESIAN_POINT('',(0.,0.628216405190687,-1.66545613819437));
#26661=CARTESIAN_POINT('',(0.,0.628216405190687,-1.66545613819437));
#26662=CARTESIAN_POINT('',(12.,0.628216405190687,-1.66545613819437));
#26663=CARTESIAN_POINT('',(12.,0.628216405190687,-1.66545613819437));
#26664=CARTESIAN_POINT('',(0.,0.628216405190687,-1.66545613819437));
#26665=CARTESIAN_POINT('Origin',(0.,1.0082031017262,-1.46694461574719));
#26666=CARTESIAN_POINT('',(0.,1.0082031017262,-1.46694461574719));
#26667=CARTESIAN_POINT('',(0.,1.0082031017262,-1.46694461574719));
#26668=CARTESIAN_POINT('',(12.,1.0082031017262,-1.46694461574719));
#26669=CARTESIAN_POINT('',(12.,1.0082031017262,-1.46694461574719));
#26670=CARTESIAN_POINT('',(0.,1.0082031017262,-1.46694461574719));
#26671=CARTESIAN_POINT('Origin',(0.,1.32970462680897,-1.18333664079281));
#26672=CARTESIAN_POINT('',(0.,1.32970462680897,-1.18333664079281));
#26673=CARTESIAN_POINT('',(0.,1.32970462680897,-1.18333664079281));
#26674=CARTESIAN_POINT('',(12.,1.32970462680897,-1.18333664079281));
#26675=CARTESIAN_POINT('',(12.,1.32970462680897,-1.18333664079281));
#26676=CARTESIAN_POINT('',(0.,1.32970462680897,-1.18333664079281));
#26677=CARTESIAN_POINT('Origin',(0.,1.57407089715261,-0.83108411772646));
#26678=CARTESIAN_POINT('',(0.,1.57407089715261,-0.83108411772646));
#26679=CARTESIAN_POINT('',(0.,1.57407089715261,-0.83108411772646));
#26680=CARTESIAN_POINT('',(12.,1.57407089715261,-0.83108411772646));
#26681=CARTESIAN_POINT('',(12.,1.57407089715261,-0.83108411772646));
#26682=CARTESIAN_POINT('',(0.,1.57407089715261,-0.83108411772646));
#26683=CARTESIAN_POINT('Origin',(0.,1.72712639277127,-0.43062097416741));
#26684=CARTESIAN_POINT('',(0.,1.72712639277127,-0.43062097416741));
#26685=CARTESIAN_POINT('',(0.,1.72712639277127,-0.43062097416741));
#26686=CARTESIAN_POINT('',(12.,1.72712639277127,-0.43062097416741));
#26687=CARTESIAN_POINT('',(12.,1.72712639277127,-0.43062097416741));
#26688=CARTESIAN_POINT('',(0.,1.72712639277127,-0.43062097416741));
#26689=CARTESIAN_POINT('Origin',(0.,2.30930382853687,-0.575774111527212));
#26690=CARTESIAN_POINT('',(0.,2.30930382853687,-0.575774111527212));
#26691=CARTESIAN_POINT('',(0.,2.30930382853687,-0.575774111527212));
#26692=CARTESIAN_POINT('',(12.,2.30930382853687,-0.575774111527212));
#26693=CARTESIAN_POINT('',(12.,2.30930382853687,-0.575774111527212));
#26694=CARTESIAN_POINT('',(0.,2.30930382853687,-0.575774111527212));
#26695=CARTESIAN_POINT('Origin',(0.,2.10465659282203,-1.11122483156684));
#26696=CARTESIAN_POINT('',(0.,2.10465659282203,-1.11122483156684));
#26697=CARTESIAN_POINT('',(0.,2.10465659282203,-1.11122483156684));
#26698=CARTESIAN_POINT('',(12.,2.10465659282203,-1.11122483156684));
#26699=CARTESIAN_POINT('',(12.,2.10465659282203,-1.11122483156684));
#26700=CARTESIAN_POINT('',(0.,2.10465659282203,-1.11122483156684));
#26701=CARTESIAN_POINT('Origin',(0.,1.77791966955357,-1.58221416016117));
#26702=CARTESIAN_POINT('',(0.,1.77791966955357,-1.58221416016117));
#26703=CARTESIAN_POINT('',(0.,1.77791966955357,-1.58221416016117));
#26704=CARTESIAN_POINT('',(12.,1.77791966955357,-1.58221416016117));
#26705=CARTESIAN_POINT('',(12.,1.77791966955357,-1.58221416016117));
#26706=CARTESIAN_POINT('',(0.,1.77791966955357,-1.58221416016117));
#26707=CARTESIAN_POINT('Origin',(0.,1.3480468438811,-1.9614203289204));
#26708=CARTESIAN_POINT('',(0.,1.3480468438811,-1.9614203289204));
#26709=CARTESIAN_POINT('',(0.,1.3480468438811,-1.9614203289204));
#26710=CARTESIAN_POINT('',(12.,1.3480468438811,-1.9614203289204));
#26711=CARTESIAN_POINT('',(12.,1.3480468438811,-1.9614203289204));
#26712=CARTESIAN_POINT('',(0.,1.3480468438811,-1.9614203289204));
#26713=CARTESIAN_POINT('Origin',(0.,0.839974744019008,-2.22684584769808));
#26714=CARTESIAN_POINT('',(0.,0.839974744019008,-2.22684584769808));
#26715=CARTESIAN_POINT('',(0.,0.839974744019008,-2.22684584769808));
#26716=CARTESIAN_POINT('',(12.,0.839974744019008,-2.22684584769808));
#26717=CARTESIAN_POINT('',(12.,0.839974744019008,-2.22684584769808));
#26718=CARTESIAN_POINT('',(0.,0.839974744019008,-2.22684584769808));
#26719=CARTESIAN_POINT('Origin',(0.,0.28317628452182,-2.36309356392937));
#26720=CARTESIAN_POINT('',(0.,0.28317628452182,-2.36309356392937));
#26721=CARTESIAN_POINT('',(0.,0.28317628452182,-2.36309356392937));
#26722=CARTESIAN_POINT('',(12.,0.28317628452182,-2.36309356392937));
#26723=CARTESIAN_POINT('',(12.,0.28317628452182,-2.36309356392937));
#26724=CARTESIAN_POINT('',(0.,0.28317628452182,-2.36309356392937));
#26725=CARTESIAN_POINT('Origin',(0.,-0.29004903730425,-2.36225984090635));
#26726=CARTESIAN_POINT('',(0.,-0.29004903730425,-2.36225984090635));
#26727=CARTESIAN_POINT('',(0.,-0.29004903730425,-2.36225984090635));
#26728=CARTESIAN_POINT('',(12.,-0.29004903730425,-2.36225984090635));
#26729=CARTESIAN_POINT('',(12.,-0.29004903730425,-2.36225984090635));
#26730=CARTESIAN_POINT('',(0.,-0.29004903730425,-2.36225984090635));
#26731=CARTESIAN_POINT('Origin',(0.,-0.846448813119406,-2.22439304233059));
#26732=CARTESIAN_POINT('',(0.,-0.846448813119406,-2.22439304233059));
#26733=CARTESIAN_POINT('',(0.,-0.846448813119406,-2.22439304233059));
#26734=CARTESIAN_POINT('',(12.,-0.846448813119406,-2.22439304233059));
#26735=CARTESIAN_POINT('',(12.,-0.846448813119406,-2.22439304233059));
#26736=CARTESIAN_POINT('',(0.,-0.846448813119406,-2.22439304233059));
#26737=CARTESIAN_POINT('Origin',(0.,-1.35374667298479,-1.95749072676798));
#26738=CARTESIAN_POINT('',(0.,-1.35374667298479,-1.95749072676798));
#26739=CARTESIAN_POINT('',(0.,-1.35374667298479,-1.95749072676798));
#26740=CARTESIAN_POINT('',(12.,-1.35374667298479,-1.95749072676798));
#26741=CARTESIAN_POINT('',(12.,-1.35374667298479,-1.95749072676798));
#26742=CARTESIAN_POINT('',(0.,-1.35374667298479,-1.95749072676798));
#26743=CARTESIAN_POINT('Origin',(0.,-1.78251461547782,-1.57703571475346));
#26744=CARTESIAN_POINT('',(0.,-1.78251461547782,-1.57703571475346));
#26745=CARTESIAN_POINT('',(0.,-1.78251461547782,-1.57703571475346));
#26746=CARTESIAN_POINT('',(12.,-1.78251461547782,-1.57703571475346));
#26747=CARTESIAN_POINT('',(12.,-1.78251461547782,-1.57703571475346));
#26748=CARTESIAN_POINT('',(0.,-1.78251461547782,-1.57703571475346));
#26749=CARTESIAN_POINT('Origin',(0.,-2.10788010590069,-1.10509794097542));
#26750=CARTESIAN_POINT('',(0.,-2.10788010590069,-1.10509794097542));
#26751=CARTESIAN_POINT('',(0.,-2.10788010590069,-1.10509794097542));
#26752=CARTESIAN_POINT('',(12.,-2.10788010590069,-1.10509794097541));
#26753=CARTESIAN_POINT('',(12.,-2.10788010590069,-1.10509794097542));
#26754=CARTESIAN_POINT('',(0.,-2.10788010590069,-1.10509794097542));
#26755=CARTESIAN_POINT('Origin',(0.,-2.31096891498389,-0.569054192479223));
#26756=CARTESIAN_POINT('',(0.,-2.31096891498389,-0.569054192479223));
#26757=CARTESIAN_POINT('',(0.,-2.31096891498389,-0.569054192479223));
#26758=CARTESIAN_POINT('',(12.,-2.31096891498389,-0.569054192479223));
#26759=CARTESIAN_POINT('',(12.,-2.31096891498389,-0.569054192479223));
#26760=CARTESIAN_POINT('',(0.,-2.31096891498389,-0.569054192479223));
#26761=CARTESIAN_POINT('Origin',(0.,-2.38,1.34839825764022E-15));
#26762=CARTESIAN_POINT('',(0.,-2.38,1.34839825764022E-15));
#26763=CARTESIAN_POINT('',(0.,-2.38,1.34839825764022E-15));
#26764=CARTESIAN_POINT('',(12.,-2.38,1.31838984174237E-15));
#26765=CARTESIAN_POINT('',(12.,-2.38,1.34839825764022E-15));
#26766=CARTESIAN_POINT('',(0.,-2.38,1.34839825764022E-15));
#26767=CARTESIAN_POINT('Origin',(0.,-2.31096891498389,0.569054192479223));
#26768=CARTESIAN_POINT('',(0.,-2.31096891498389,0.569054192479223));
#26769=CARTESIAN_POINT('',(0.,-2.31096891498389,0.569054192479223));
#26770=CARTESIAN_POINT('',(12.,-2.31096891498389,0.569054192479223));
#26771=CARTESIAN_POINT('',(12.,-2.31096891498389,0.569054192479223));
#26772=CARTESIAN_POINT('',(0.,-2.31096891498389,0.569054192479223));
#26773=CARTESIAN_POINT('Origin',(0.,-2.10788010590069,1.10509794097542));
#26774=CARTESIAN_POINT('',(0.,-2.10788010590069,1.10509794097542));
#26775=CARTESIAN_POINT('',(0.,-2.10788010590069,1.10509794097542));
#26776=CARTESIAN_POINT('',(12.,-2.10788010590069,1.10509794097542));
#26777=CARTESIAN_POINT('',(12.,-2.10788010590069,1.10509794097542));
#26778=CARTESIAN_POINT('',(0.,-2.10788010590069,1.10509794097542));
#26779=CARTESIAN_POINT('Origin',(0.,-1.78251461547783,1.57703571475345));
#26780=CARTESIAN_POINT('',(0.,-1.78251461547783,1.57703571475345));
#26781=CARTESIAN_POINT('',(0.,-1.78251461547783,1.57703571475345));
#26782=CARTESIAN_POINT('',(12.,-1.78251461547783,1.57703571475345));
#26783=CARTESIAN_POINT('',(12.,-1.78251461547783,1.57703571475345));
#26784=CARTESIAN_POINT('',(0.,-1.78251461547783,1.57703571475345));
#26785=CARTESIAN_POINT('Origin',(0.,-1.35374667298479,1.95749072676798));
#26786=CARTESIAN_POINT('',(0.,-1.35374667298479,1.95749072676798));
#26787=CARTESIAN_POINT('',(0.,-1.35374667298479,1.95749072676798));
#26788=CARTESIAN_POINT('',(12.,-1.35374667298479,1.95749072676798));
#26789=CARTESIAN_POINT('',(12.,-1.35374667298479,1.95749072676798));
#26790=CARTESIAN_POINT('',(0.,-1.35374667298479,1.95749072676798));
#26791=CARTESIAN_POINT('Origin',(0.,-0.846448813119406,2.22439304233059));
#26792=CARTESIAN_POINT('',(0.,-0.846448813119406,2.22439304233059));
#26793=CARTESIAN_POINT('',(0.,-0.846448813119406,2.22439304233059));
#26794=CARTESIAN_POINT('',(12.,-0.846448813119405,2.22439304233059));
#26795=CARTESIAN_POINT('',(12.,-0.846448813119406,2.22439304233059));
#26796=CARTESIAN_POINT('',(0.,-0.846448813119406,2.22439304233059));
#26797=CARTESIAN_POINT('Origin',(0.,-0.290049037304251,2.36225984090635));
#26798=CARTESIAN_POINT('',(0.,-0.290049037304251,2.36225984090635));
#26799=CARTESIAN_POINT('',(0.,-0.290049037304251,2.36225984090635));
#26800=CARTESIAN_POINT('',(12.,-0.290049037304251,2.36225984090635));
#26801=CARTESIAN_POINT('',(12.,-0.290049037304251,2.36225984090635));
#26802=CARTESIAN_POINT('',(0.,-0.290049037304251,2.36225984090635));
#26803=CARTESIAN_POINT('Origin',(0.,0.283176284521821,2.36309356392937));
#26804=CARTESIAN_POINT('',(0.,0.283176284521821,2.36309356392937));
#26805=CARTESIAN_POINT('',(0.,0.283176284521821,2.36309356392937));
#26806=CARTESIAN_POINT('',(12.,0.283176284521821,2.36309356392937));
#26807=CARTESIAN_POINT('',(12.,0.283176284521821,2.36309356392937));
#26808=CARTESIAN_POINT('',(0.,0.283176284521821,2.36309356392937));
#26809=CARTESIAN_POINT('Origin',(0.,0.839974744019008,2.22684584769809));
#26810=CARTESIAN_POINT('',(0.,0.839974744019008,2.22684584769809));
#26811=CARTESIAN_POINT('',(0.,0.839974744019008,2.22684584769809));
#26812=CARTESIAN_POINT('',(12.,0.839974744019008,2.22684584769809));
#26813=CARTESIAN_POINT('',(12.,0.839974744019008,2.22684584769809));
#26814=CARTESIAN_POINT('',(0.,0.839974744019008,2.22684584769809));
#26815=CARTESIAN_POINT('Origin',(0.,1.3480468438811,1.9614203289204));
#26816=CARTESIAN_POINT('',(0.,1.3480468438811,1.9614203289204));
#26817=CARTESIAN_POINT('',(0.,1.3480468438811,1.9614203289204));
#26818=CARTESIAN_POINT('',(12.,1.3480468438811,1.9614203289204));
#26819=CARTESIAN_POINT('',(12.,1.3480468438811,1.9614203289204));
#26820=CARTESIAN_POINT('',(0.,1.3480468438811,1.9614203289204));
#26821=CARTESIAN_POINT('Origin',(0.,1.77791966955357,1.58221416016117));
#26822=CARTESIAN_POINT('',(0.,1.77791966955357,1.58221416016117));
#26823=CARTESIAN_POINT('',(0.,1.77791966955357,1.58221416016117));
#26824=CARTESIAN_POINT('',(12.,1.77791966955357,1.58221416016117));
#26825=CARTESIAN_POINT('',(12.,1.77791966955357,1.58221416016117));
#26826=CARTESIAN_POINT('',(0.,1.77791966955357,1.58221416016117));
#26827=CARTESIAN_POINT('Origin',(0.,2.10465659282203,1.11122483156684));
#26828=CARTESIAN_POINT('',(0.,2.10465659282203,1.11122483156684));
#26829=CARTESIAN_POINT('',(0.,2.10465659282203,1.11122483156684));
#26830=CARTESIAN_POINT('',(12.,2.10465659282203,1.11122483156684));
#26831=CARTESIAN_POINT('',(12.,2.10465659282203,1.11122483156684));
#26832=CARTESIAN_POINT('',(0.,2.10465659282203,1.11122483156684));
#26833=CARTESIAN_POINT('Origin',(0.,2.30930382853687,0.575774111527209));
#26834=CARTESIAN_POINT('',(0.,2.30930382853687,0.575774111527209));
#26835=CARTESIAN_POINT('',(0.,2.30930382853687,0.575774111527209));
#26836=CARTESIAN_POINT('',(12.,2.30930382853687,0.575774111527209));
#26837=CARTESIAN_POINT('',(12.,2.30930382853687,0.575774111527209));
#26838=CARTESIAN_POINT('',(0.,2.30930382853687,0.575774111527209));
#26839=CARTESIAN_POINT('Origin',(0.,1.72712639277127,0.430620974167409));
#26840=CARTESIAN_POINT('',(0.,1.72712639277127,0.430620974167409));
#26841=CARTESIAN_POINT('',(12.,1.72712639277127,0.430620974167409));
#26842=CARTESIAN_POINT('Origin',(12.,-0.0353480857315641,0.));
#26843=CARTESIAN_POINT('Origin',(0.,-0.0353480857315641,0.));
#26844=CARTESIAN_POINT('',(0.,0.,0.));
#26845=CARTESIAN_POINT('Origin',(-5.05,-72.25,-2.));
#26846=CARTESIAN_POINT('',(-4.8,-72.5,-4.));
#26847=CARTESIAN_POINT('',(-5.3,-72.,-4.));
#26848=CARTESIAN_POINT('',(-4.8,-72.5,-4.));
#26849=CARTESIAN_POINT('',(-5.3,-72.,4.));
#26850=CARTESIAN_POINT('',(-5.3,-72.,-2.));
#26851=CARTESIAN_POINT('',(-4.8,-72.5,4.));
#26852=CARTESIAN_POINT('',(-5.3,-72.,4.));
#26853=CARTESIAN_POINT('',(-4.8,-72.5,-2.));
#26854=CARTESIAN_POINT('Origin',(2.2,-72.25,-4.));
#26855=CARTESIAN_POINT('',(2.2,-72.5,-11.));
#26856=CARTESIAN_POINT('',(2.2,-72.,-11.5));
#26857=CARTESIAN_POINT('',(2.2,-72.5,-11.));
#26858=CARTESIAN_POINT('Origin',(2.2,-72.,-4.));
#26859=CARTESIAN_POINT('Origin',(2.2,-72.5,-4.));
#26860=CARTESIAN_POINT('Origin',(21.7,-72.25,-11.25));
#26861=CARTESIAN_POINT('',(28.2,-72.5,-11.));
#26862=CARTESIAN_POINT('',(28.2,-72.,-11.5));
#26863=CARTESIAN_POINT('',(28.2,-72.5,-11.));
#26864=CARTESIAN_POINT('',(21.7,-72.,-11.5));
#26865=CARTESIAN_POINT('',(21.7,-72.5,-11.));
#26866=CARTESIAN_POINT('Origin',(28.2,-72.25,-3.99999999999999));
#26867=CARTESIAN_POINT('',(35.2,-72.5,-4.));
#26868=CARTESIAN_POINT('',(35.7,-72.,-4.));
#26869=CARTESIAN_POINT('',(35.2,-72.5,-4.));
#26870=CARTESIAN_POINT('Origin',(28.2,-72.,-3.99999999999999));
#26871=CARTESIAN_POINT('Origin',(28.2,-72.5,-3.99999999999999));
#26872=CARTESIAN_POINT('Origin',(35.45,-72.25,2.));
#26873=CARTESIAN_POINT('',(35.2,-72.5,4.));
#26874=CARTESIAN_POINT('',(35.7,-72.,4.));
#26875=CARTESIAN_POINT('',(35.2,-72.5,4.));
#26876=CARTESIAN_POINT('',(35.7,-72.,2.));
#26877=CARTESIAN_POINT('',(35.2,-72.5,2.));
#26878=CARTESIAN_POINT('Origin',(28.2,-72.25,3.99999999999999));
#26879=CARTESIAN_POINT('',(28.2,-72.5,11.));
#26880=CARTESIAN_POINT('',(28.2,-72.,11.5));
#26881=CARTESIAN_POINT('',(28.2,-72.5,11.));
#26882=CARTESIAN_POINT('Origin',(28.2,-72.,3.99999999999999));
#26883=CARTESIAN_POINT('Origin',(28.2,-72.5,3.99999999999999));
#26884=CARTESIAN_POINT('Origin',(8.7,-72.25,11.25));
#26885=CARTESIAN_POINT('',(2.2,-72.5,11.));
#26886=CARTESIAN_POINT('',(2.2,-72.,11.5));
#26887=CARTESIAN_POINT('',(2.2,-72.5,11.));
#26888=CARTESIAN_POINT('',(8.7,-72.,11.5));
#26889=CARTESIAN_POINT('',(8.7,-72.5,11.));
#26890=CARTESIAN_POINT('Origin',(2.2,-72.25,4.));
#26891=CARTESIAN_POINT('Origin',(2.2,-72.,4.));
#26892=CARTESIAN_POINT('Origin',(2.2,-72.5,4.));
#26893=CARTESIAN_POINT('Origin',(28.2,-72.,-3.99999999999999));
#26894=CARTESIAN_POINT('',(28.2,-73.5,-11.));
#26895=CARTESIAN_POINT('',(28.2,-72.,-11.));
#26896=CARTESIAN_POINT('',(35.2,-73.5,-4.));
#26897=CARTESIAN_POINT('Origin',(28.2,-73.5,-3.99999999999999));
#26898=CARTESIAN_POINT('',(35.2,-72.,-4.));
#26899=CARTESIAN_POINT('Origin',(28.2,-72.,-11.));
#26900=CARTESIAN_POINT('',(2.2,-73.5,-11.));
#26901=CARTESIAN_POINT('',(2.2,-72.,-11.));
#26902=CARTESIAN_POINT('',(21.7,-73.5,-11.));
#26903=CARTESIAN_POINT('Origin',(2.2,-72.,-4.));
#26904=CARTESIAN_POINT('',(-4.8,-73.5,-4.));
#26905=CARTESIAN_POINT('',(-4.8,-72.,-4.));
#26906=CARTESIAN_POINT('Origin',(2.2,-73.5,-4.));
#26907=CARTESIAN_POINT('Origin',(-4.8,-72.,-4.));
#26908=CARTESIAN_POINT('',(-4.8,-73.5,4.));
#26909=CARTESIAN_POINT('',(-4.8,-72.,4.));
#26910=CARTESIAN_POINT('',(-4.8,-73.5,-2.));
#26911=CARTESIAN_POINT('Origin',(15.2,-72.,0.));
#26912=CARTESIAN_POINT('',(37.5,-72.,-4.));
#26913=CARTESIAN_POINT('',(37.5,-72.,4.));
#26914=CARTESIAN_POINT('',(37.5,-72.,2.));
#26915=CARTESIAN_POINT('',(28.2,-72.,-13.3));
#26916=CARTESIAN_POINT('Origin',(28.2,-72.,-4.));
#26917=CARTESIAN_POINT('',(2.2,-72.,-13.3));
#26918=CARTESIAN_POINT('',(21.7,-72.,-13.3));
#26919=CARTESIAN_POINT('',(-7.1,-72.,-4.));
#26920=CARTESIAN_POINT('Origin',(2.20000000000001,-72.,-3.99999999999999));
#26921=CARTESIAN_POINT('',(-7.1,-72.,4.));
#26922=CARTESIAN_POINT('',(-7.1,-72.,-2.));
#26923=CARTESIAN_POINT('',(2.2,-72.,13.3));
#26924=CARTESIAN_POINT('Origin',(2.2,-72.,3.99999999999999));
#26925=CARTESIAN_POINT('',(28.2,-72.,13.3));
#26926=CARTESIAN_POINT('',(8.7,-72.,13.3));
#26927=CARTESIAN_POINT('Origin',(28.2,-72.,4.));
#26928=CARTESIAN_POINT('Origin',(28.2,-32.25,-4.));
#26929=CARTESIAN_POINT('',(37.5,-32.5,-4.));
#26930=CARTESIAN_POINT('',(38.,-32.,-4.));
#26931=CARTESIAN_POINT('',(37.5,-32.5,-4.));
#26932=CARTESIAN_POINT('',(28.2,-32.,-13.8));
#26933=CARTESIAN_POINT('Origin',(28.2,-32.,-4.));
#26934=CARTESIAN_POINT('',(28.2,-32.5,-13.3));
#26935=CARTESIAN_POINT('',(28.2,-32.,-13.8));
#26936=CARTESIAN_POINT('Origin',(28.2,-32.5,-4.));
#26937=CARTESIAN_POINT('Origin',(37.75,-32.25,2.));
#26938=CARTESIAN_POINT('',(37.5,-32.5,4.));
#26939=CARTESIAN_POINT('',(38.,-32.,4.));
#26940=CARTESIAN_POINT('',(37.5,-32.5,4.));
#26941=CARTESIAN_POINT('',(38.,-32.,2.));
#26942=CARTESIAN_POINT('',(37.5,-32.5,2.));
#26943=CARTESIAN_POINT('Origin',(28.2,-32.25,4.));
#26944=CARTESIAN_POINT('',(28.2,-32.5,13.3));
#26945=CARTESIAN_POINT('',(28.2,-32.,13.8));
#26946=CARTESIAN_POINT('',(28.2,-32.5,13.3));
#26947=CARTESIAN_POINT('Origin',(28.2,-32.,4.));
#26948=CARTESIAN_POINT('Origin',(28.2,-32.5,4.));
#26949=CARTESIAN_POINT('Origin',(8.7,-32.25,13.55));
#26950=CARTESIAN_POINT('',(2.2,-32.5,13.3));
#26951=CARTESIAN_POINT('',(2.2,-32.,13.8));
#26952=CARTESIAN_POINT('',(2.2,-32.5,13.3));
#26953=CARTESIAN_POINT('',(8.7,-32.,13.8));
#26954=CARTESIAN_POINT('',(8.7,-32.5,13.3));
#26955=CARTESIAN_POINT('Origin',(2.2,-32.25,3.99999999999999));
#26956=CARTESIAN_POINT('',(-7.1,-32.5,4.));
#26957=CARTESIAN_POINT('',(-7.6,-32.,4.));
#26958=CARTESIAN_POINT('',(-7.1,-32.5,4.));
#26959=CARTESIAN_POINT('Origin',(2.2,-32.,3.99999999999999));
#26960=CARTESIAN_POINT('Origin',(2.2,-32.5,3.99999999999999));
#26961=CARTESIAN_POINT('Origin',(-7.35,-32.25,-2.));
#26962=CARTESIAN_POINT('',(-7.1,-32.5,-4.));
#26963=CARTESIAN_POINT('',(-7.6,-32.,-4.));
#26964=CARTESIAN_POINT('',(-7.1,-32.5,-4.));
#26965=CARTESIAN_POINT('',(-7.6,-32.,-2.));
#26966=CARTESIAN_POINT('',(-7.1,-32.5,-2.));
#26967=CARTESIAN_POINT('Origin',(2.20000000000001,-32.25,-3.99999999999999));
#26968=CARTESIAN_POINT('',(2.2,-32.5,-13.3));
#26969=CARTESIAN_POINT('',(2.2,-32.,-13.8));
#26970=CARTESIAN_POINT('',(2.2,-32.5,-13.3));
#26971=CARTESIAN_POINT('Origin',(2.20000000000001,-32.,-3.99999999999999));
#26972=CARTESIAN_POINT('Origin',(2.20000000000001,-32.5,-3.99999999999999));
#26973=CARTESIAN_POINT('Origin',(21.7,-32.25,-13.55));
#26974=CARTESIAN_POINT('',(21.7,-32.,-13.8));
#26975=CARTESIAN_POINT('',(21.7,-32.5,-13.3));
#26976=CARTESIAN_POINT('Origin',(2.2,-32.,13.3));
#26977=CARTESIAN_POINT('',(28.2,-32.,13.3));
#26978=CARTESIAN_POINT('',(2.2,-32.,13.3));
#26979=CARTESIAN_POINT('Origin',(28.2,-32.,4.));
#26980=CARTESIAN_POINT('',(37.5,-32.,4.));
#26981=CARTESIAN_POINT('Origin',(37.5,-32.,4.));
#26982=CARTESIAN_POINT('',(37.5,-32.,-4.));
#26983=CARTESIAN_POINT('Origin',(28.2,-32.,-4.));
#26984=CARTESIAN_POINT('',(28.2,-32.,-13.3));
#26985=CARTESIAN_POINT('Origin',(15.2,-32.,0.));
#26986=CARTESIAN_POINT('',(41.7,-32.,20.));
#26987=CARTESIAN_POINT('',(35.2,-32.,26.5));
#26988=CARTESIAN_POINT('Origin',(35.2,-32.,20.));
#26989=CARTESIAN_POINT('',(41.7,-32.,-20.));
#26990=CARTESIAN_POINT('',(41.7,-32.,-10.));
#26991=CARTESIAN_POINT('',(35.2,-32.,-26.5));
#26992=CARTESIAN_POINT('Origin',(35.2,-32.,-20.));
#26993=CARTESIAN_POINT('',(-4.8,-32.,-26.5));
#26994=CARTESIAN_POINT('',(5.2,-32.,-26.5));
#26995=CARTESIAN_POINT('',(-11.3,-32.,-20.));
#26996=CARTESIAN_POINT('Origin',(-4.79999999999999,-32.,-20.));
#26997=CARTESIAN_POINT('',(-11.3,-32.,20.));
#26998=CARTESIAN_POINT('',(-11.3,-32.,10.));
#26999=CARTESIAN_POINT('',(-4.8,-32.,26.5));
#27000=CARTESIAN_POINT('Origin',(-4.79999999999999,-32.,20.));
#27001=CARTESIAN_POINT('',(25.2,-32.,26.5));
#27002=CARTESIAN_POINT('Origin',(35.2,-32.25,20.));
#27003=CARTESIAN_POINT('',(42.2,-32.5,20.));
#27004=CARTESIAN_POINT('',(42.2,-32.5,20.));
#27005=CARTESIAN_POINT('',(35.2,-32.5,27.));
#27006=CARTESIAN_POINT('',(35.2,-32.,26.5));
#27007=CARTESIAN_POINT('Origin',(35.2,-32.5,20.));
#27008=CARTESIAN_POINT('Origin',(41.95,-32.25,-10.));
#27009=CARTESIAN_POINT('',(42.2,-32.5,-20.));
#27010=CARTESIAN_POINT('',(42.2,-32.5,-10.));
#27011=CARTESIAN_POINT('',(42.2,-32.5,-20.));
#27012=CARTESIAN_POINT('Origin',(35.2,-32.25,-20.));
#27013=CARTESIAN_POINT('',(35.2,-32.5,-27.));
#27014=CARTESIAN_POINT('',(35.2,-32.5,-27.));
#27015=CARTESIAN_POINT('Origin',(35.2,-32.5,-20.));
#27016=CARTESIAN_POINT('Origin',(5.2,-32.25,-26.75));
#27017=CARTESIAN_POINT('',(-4.8,-32.5,-27.));
#27018=CARTESIAN_POINT('',(5.2,-32.5,-27.));
#27019=CARTESIAN_POINT('',(-4.8,-32.5,-27.));
#27020=CARTESIAN_POINT('Origin',(-4.79999999999999,-32.25,-20.));
#27021=CARTESIAN_POINT('',(-11.8,-32.5,-20.));
#27022=CARTESIAN_POINT('',(-11.8,-32.5,-20.));
#27023=CARTESIAN_POINT('Origin',(-4.79999999999999,-32.5,-20.));
#27024=CARTESIAN_POINT('Origin',(-11.55,-32.25,10.));
#27025=CARTESIAN_POINT('',(-11.8,-32.5,20.));
#27026=CARTESIAN_POINT('',(-11.8,-32.5,10.));
#27027=CARTESIAN_POINT('',(-11.8,-32.5,20.));
#27028=CARTESIAN_POINT('Origin',(-4.79999999999999,-32.25,20.));
#27029=CARTESIAN_POINT('',(-4.8,-32.5,27.));
#27030=CARTESIAN_POINT('',(-4.8,-32.5,27.));
#27031=CARTESIAN_POINT('Origin',(-4.79999999999999,-32.5,20.));
#27032=CARTESIAN_POINT('Origin',(25.2,-32.25,26.75));
#27033=CARTESIAN_POINT('',(25.2,-32.5,27.));
#27034=CARTESIAN_POINT('Origin',(-4.8,-32.,-27.));
#27035=CARTESIAN_POINT('',(35.2,-71.9490268349807,-27.));
#27036=CARTESIAN_POINT('',(35.2,-32.,-27.));
#27037=CARTESIAN_POINT('',(34.0097619285762,-72.5,-27.));
#27038=CARTESIAN_POINT('',(34.6048809642881,-72.2245134174903,-27.));
#27039=CARTESIAN_POINT('',(-3.60976192857618,-72.5,-27.));
#27040=CARTESIAN_POINT('',(5.2,-72.5,-27.));
#27041=CARTESIAN_POINT('',(-4.8,-71.9490268349807,-27.));
#27042=CARTESIAN_POINT('',(-4.20488096428809,-72.2245134174903,-27.));
#27043=CARTESIAN_POINT('',(-4.8,-32.,-27.));
#27044=CARTESIAN_POINT('Origin',(35.2,-32.,-20.));
#27045=CARTESIAN_POINT('',(42.2,-71.9490268349807,-20.));
#27046=CARTESIAN_POINT('',(42.2,-32.,-20.));
#27047=CARTESIAN_POINT('',(42.1968209160836,-72.0466857368163,-20.2109432820811));
#27048=CARTESIAN_POINT('Ctrl Pts',(42.1968209160836,-72.0466857368163,-20.2109432820811));
#27049=CARTESIAN_POINT('Ctrl Pts',(42.1968440264343,-72.0463307309993,-20.2101767301278));
#27050=CARTESIAN_POINT('Ctrl Pts',(42.196867151744,-72.0459737810207,-20.2094059772172));
#27051=CARTESIAN_POINT('Ctrl Pts',(42.1968938349779,-72.0455591055399,-20.2085105801841));
#27052=CARTESIAN_POINT('Ctrl Pts',(42.1969215748069,-72.0451280098565,-20.2075797274724));
#27053=CARTESIAN_POINT('Ctrl Pts',(42.1969531556842,-72.0446346198902,-20.2065143654833));
#27054=CARTESIAN_POINT('Ctrl Pts',(42.1969907706432,-72.0440407131694,-20.2052319554396));
#27055=CARTESIAN_POINT('Ctrl Pts',(42.1970302352795,-72.0434176016909,-20.2038864841889));
#27056=CARTESIAN_POINT('Ctrl Pts',(42.1970763351041,-72.0426839627648,-20.2023023485086));
#27057=CARTESIAN_POINT('Ctrl Pts',(42.1971297471362,-72.0418204588819,-20.2004377752349));
#27058=CARTESIAN_POINT('Ctrl Pts',(42.1971866204212,-72.0409009974715,-20.1984523722667));
#27059=CARTESIAN_POINT('Ctrl Pts',(42.1972517663276,-72.039834454825,-20.1961493535318));
#27060=CARTESIAN_POINT('Ctrl Pts',(42.1973241283667,-72.0386228526127,-20.1935330529333));
#27061=CARTESIAN_POINT('Ctrl Pts',(42.1974033531205,-72.0372963437394,-20.1906686260413));
#27062=CARTESIAN_POINT('Ctrl Pts',(42.1974911870066,-72.0357962057728,-20.1874292153276));
#27063=CARTESIAN_POINT('Ctrl Pts',(42.197584514987,-72.0341515121676,-20.1838775560355));
#27064=CARTESIAN_POINT('Ctrl Pts',(42.1976993757062,-72.0321273529655,-20.1795064538336));
#27065=CARTESIAN_POINT('Ctrl Pts',(42.197822445902,-72.0298846925147,-20.1746633732515));
#27066=CARTESIAN_POINT('Ctrl Pts',(42.1979466024095,-72.027511696443,-20.1695386381502));
#27067=CARTESIAN_POINT('Ctrl Pts',(42.1980821533145,-72.024920919917,-20.1639435832062));
#27068=CARTESIAN_POINT('Ctrl Pts',(42.1982187728114,-72.0221774130799,-20.1580184730275));
#27069=CARTESIAN_POINT('Ctrl Pts',(42.1983487795842,-72.0194065699845,-20.1520340727998));
#27070=CARTESIAN_POINT('Ctrl Pts',(42.1984473485597,-72.0173057627784,-20.1474967999592));
#27071=CARTESIAN_POINT('Ctrl Pts',(42.198542156045,-72.0151898308564,-20.1429267194319));
#27072=CARTESIAN_POINT('Ctrl Pts',(42.198631372502,-72.0131013188952,-20.1384157210408));
#27073=CARTESIAN_POINT('Ctrl Pts',(42.1987118838834,-72.0112165883326,-20.1343448721814));
#27074=CARTESIAN_POINT('Ctrl Pts',(42.1987878612489,-72.0093544513594,-20.1303227080405));
#27075=CARTESIAN_POINT('Ctrl Pts',(42.198859022311,-72.0075300311515,-20.1263819046223));
#27076=CARTESIAN_POINT('Ctrl Pts',(42.1989256149734,-72.0058227351212,-20.1226940930081));
#27077=CARTESIAN_POINT('Ctrl Pts',(42.1989880057221,-72.0041486403603,-20.1190779023671));
#27078=CARTESIAN_POINT('Ctrl Pts',(42.1990467044472,-72.0025022857799,-20.1155215519585));
#27079=CARTESIAN_POINT('Ctrl Pts',(42.1991060919784,-72.0008366118852,-20.1119234691961));
#27080=CARTESIAN_POINT('Ctrl Pts',(42.199161711364,-71.999199728262,-20.1083874932512));
#27081=CARTESIAN_POINT('Ctrl Pts',(42.1992146913247,-71.9975625728967,-20.1048508690683));
#27082=CARTESIAN_POINT('Ctrl Pts',(42.1992663579433,-71.9959660016516,-20.1014019157222));
#27083=CARTESIAN_POINT('Ctrl Pts',(42.19931563984,-71.9943651666196,-20.0979436948257));
#27084=CARTESIAN_POINT('Ctrl Pts',(42.1993631272831,-71.9927356970358,-20.0944235798369));
#27085=CARTESIAN_POINT('Ctrl Pts',(42.1994134018495,-71.9910105909616,-20.0906968629903));
#27086=CARTESIAN_POINT('Ctrl Pts',(42.1994616361791,-71.9892535447084,-20.0869011062894));
#27087=CARTESIAN_POINT('Ctrl Pts',(42.1995075723881,-71.9874609701946,-20.0830285738872));
#27088=CARTESIAN_POINT('Ctrl Pts',(42.1995572904834,-71.985520814653,-20.078837219418));
#27089=CARTESIAN_POINT('Ctrl Pts',(42.1996042772797,-71.9835392694509,-20.0745564223781));
#27090=CARTESIAN_POINT('Ctrl Pts',(42.1996476627856,-71.9815377443591,-20.0702324487676));
#27091=CARTESIAN_POINT('Ctrl Pts',(42.1996984016497,-71.9791969831448,-20.0651756099797));
#27092=CARTESIAN_POINT('Ctrl Pts',(42.1997441440131,-71.976829265232,-20.0600605172026));
#27093=CARTESIAN_POINT('Ctrl Pts',(42.1997837204606,-71.9744988699025,-20.0550260554195));
#27094=CARTESIAN_POINT('Ctrl Pts',(42.1998416179811,-71.9710896677196,-20.0476609968461));
#27095=CARTESIAN_POINT('Ctrl Pts',(42.1998859839155,-71.9677638296965,-20.0404760377688));
#27096=CARTESIAN_POINT('Ctrl Pts',(42.199917487043,-71.9647604963968,-20.033987859449));
#27097=CARTESIAN_POINT('Ctrl Pts',(42.1999376069614,-71.962842375057,-20.0298440924906));
#27098=CARTESIAN_POINT('Ctrl Pts',(42.1999526242593,-71.9610565580335,-20.0259861725222));
#27099=CARTESIAN_POINT('Ctrl Pts',(42.1999637788496,-71.9594514906783,-20.022518765367));
#27100=CARTESIAN_POINT('Ctrl Pts',(42.1999740893287,-71.9579678850109,-20.0193137503938));
#27101=CARTESIAN_POINT('Ctrl Pts',(42.1999811326703,-71.9566391654817,-20.0164433694763));
#27102=CARTESIAN_POINT('Ctrl Pts',(42.1999861098761,-71.9554826093195,-20.0139449468308));
#27103=CARTESIAN_POINT('Ctrl Pts',(42.1999904546681,-71.9544730074947,-20.0117639787599));
#27104=CARTESIAN_POINT('Ctrl Pts',(42.1999932364772,-71.9535945583467,-20.00986636539));
#27105=CARTESIAN_POINT('Ctrl Pts',(42.1999951540824,-71.9528401206128,-20.0082366754871));
#27106=CARTESIAN_POINT('Ctrl Pts',(42.1999969972036,-71.952114986876,-20.0066702862729));
#27107=CARTESIAN_POINT('Ctrl Pts',(42.1999980448829,-71.9515045768435,-20.0053517545771));
#27108=CARTESIAN_POINT('Ctrl Pts',(42.1999987249728,-71.9509829203972,-20.0042249709246));
#27109=CARTESIAN_POINT('Ctrl Pts',(42.1999993730205,-71.9504858415435,-20.0031512751422));
#27110=CARTESIAN_POINT('Ctrl Pts',(42.1999996854038,-71.9500694193736,-20.0022518343658));
#27111=CARTESIAN_POINT('Ctrl Pts',(42.1999998528112,-71.9496914618382,-20.001435493955));
#27112=CARTESIAN_POINT('Ctrl Pts',(42.1999999551045,-71.9494605131145,-20.0009366739598));
#27113=CARTESIAN_POINT('Ctrl Pts',(42.2,-71.9492435363225,-20.0004680394446));
#27114=CARTESIAN_POINT('Ctrl Pts',(42.2,-71.9490268349807,-20.));
#27115=CARTESIAN_POINT('',(41.0736851473658,-73.4473505177094,-23.8078632839972));
#27116=CARTESIAN_POINT('Ctrl Pts',(41.0736851473658,-73.4473505177094,-23.8078632839972));
#27117=CARTESIAN_POINT('Ctrl Pts',(41.4091108998595,-73.3524777845863,-23.2904641250657));
#27118=CARTESIAN_POINT('Ctrl Pts',(41.9708821659981,-72.9316902782726,-22.1114790525524));
#27119=CARTESIAN_POINT('Ctrl Pts',(42.1783555363975,-72.3303386029005,-20.8234252418586));
#27120=CARTESIAN_POINT('Ctrl Pts',(42.1968209160836,-72.0466857368163,-20.2109432820811));
#27121=CARTESIAN_POINT('',(40.7,-73.5,-24.3301270189222));
#27122=CARTESIAN_POINT('Ctrl Pts',(40.7,-73.5,-24.3301270189222));
#27123=CARTESIAN_POINT('Ctrl Pts',(40.8292080416589,-73.5,-24.1660107641291));
#27124=CARTESIAN_POINT('Ctrl Pts',(40.9547480121633,-73.4809910208687,-23.9913255651788));
#27125=CARTESIAN_POINT('Ctrl Pts',(41.0736851473658,-73.4473505177094,-23.8078632839972));
#27126=CARTESIAN_POINT('',(39.5301270189222,-73.5,-25.5));
#27127=CARTESIAN_POINT('Origin',(35.2,-73.5,-20.));
#27128=CARTESIAN_POINT('',(39.0078632855922,-73.4473505180018,-25.8736851463318));
#27129=CARTESIAN_POINT('Ctrl Pts',(39.0078632855922,-73.4473505180018,-25.8736851463318));
#27130=CARTESIAN_POINT('Ctrl Pts',(39.195551811226,-73.4817659650606,-25.7520081704499));
#27131=CARTESIAN_POINT('Ctrl Pts',(39.3719134220716,-73.5,-25.6245609037243));
#27132=CARTESIAN_POINT('Ctrl Pts',(39.5301270189222,-73.5,-25.5));
#27133=CARTESIAN_POINT('',(35.4109442661894,-72.0466861925664,-26.9968208864142));
#27134=CARTESIAN_POINT('Ctrl Pts',(35.4109442661894,-72.0466861925664,-26.9968208864142));
#27135=CARTESIAN_POINT('Ctrl Pts',(35.7966135491349,-72.2252974952159,-26.9851935023203));
#27136=CARTESIAN_POINT('Ctrl Pts',(36.2129500341219,-72.4189119678641,-26.93930292622));
#27137=CARTESIAN_POINT('Ctrl Pts',(37.155472782663,-72.8367867066598,-26.7392783613268));
#27138=CARTESIAN_POINT('Ctrl Pts',(37.926965678302,-73.1628447118167,-26.4889617424396));
#27139=CARTESIAN_POINT('Ctrl Pts',(38.7159981118503,-73.3938327528572,-26.0628990132224));
#27140=CARTESIAN_POINT('Ctrl Pts',(39.0078632855927,-73.4473505180019,-25.8736851463315));
#27141=CARTESIAN_POINT('Ctrl Pts',(35.2,-71.9490268349807,-27.));
#27142=CARTESIAN_POINT('Ctrl Pts',(35.2007669707035,-71.9493819403517,-27.));
#27143=CARTESIAN_POINT('Ctrl Pts',(35.2015381410139,-71.9497389896615,-26.9999998883361));
#27144=CARTESIAN_POINT('Ctrl Pts',(35.2024340110129,-71.9501537584991,-26.9999995768279));
#27145=CARTESIAN_POINT('Ctrl Pts',(35.2033653543852,-71.9505849507574,-26.999999252985));
#27146=CARTESIAN_POINT('Ctrl Pts',(35.2044312667571,-71.9510784307137,-26.999998715007));
#27147=CARTESIAN_POINT('Ctrl Pts',(35.2057143192196,-71.9516724170336,-26.9999976676107));
#27148=CARTESIAN_POINT('Ctrl Pts',(35.2070604622019,-71.9522956109712,-26.9999965687117));
#27149=CARTESIAN_POINT('Ctrl Pts',(35.2086453700289,-71.9530293205579,-26.9999949098187));
#27150=CARTESIAN_POINT('Ctrl Pts',(35.2105108197961,-71.953892881673,-26.9999921087575));
#27151=CARTESIAN_POINT('Ctrl Pts',(35.2124971503262,-71.9548124013714,-26.9999891261881));
#27152=CARTESIAN_POINT('Ctrl Pts',(35.2148012127258,-71.9558789862511,-26.9999848410617));
#27153=CARTESIAN_POINT('Ctrl Pts',(35.2174186444992,-71.9570906156705,-26.9999783278824));
#27154=CARTESIAN_POINT('Ctrl Pts',(35.2202842926812,-71.9584171463859,-26.9999711970451));
#27155=CARTESIAN_POINT('Ctrl Pts',(35.2235250241412,-71.9599172861367,-26.9999613711321));
#27156=CARTESIAN_POINT('Ctrl Pts',(35.2270780387911,-71.9615619664984,-26.9999476269337));
#27157=CARTESIAN_POINT('Ctrl Pts',(35.2314506214448,-71.9635860225548,-26.9999307123839));
#27158=CARTESIAN_POINT('Ctrl Pts',(35.2362951915127,-71.9658285383685,-26.9999077806186));
#27159=CARTESIAN_POINT('Ctrl Pts',(35.2414213179411,-71.968201373194,-26.9998774471001));
#27160=CARTESIAN_POINT('Ctrl Pts',(35.2470187031861,-71.9707923492119,-26.9998443249382));
#27161=CARTESIAN_POINT('Ctrl Pts',(35.2529461190972,-71.9735360807742,-26.9998023221268));
#27162=CARTESIAN_POINT('Ctrl Pts',(35.2589325903827,-71.9763071508733,-26.9997519205891));
#27163=CARTESIAN_POINT('Ctrl Pts',(35.2634711104776,-71.9784079806826,-26.9997137096998));
#27164=CARTESIAN_POINT('Ctrl Pts',(35.2680423000474,-71.9805239342997,-26.9996707497673));
#27165=CARTESIAN_POINT('Ctrl Pts',(35.2725542349323,-71.9826124675568,-26.9996239815431));
#27166=CARTESIAN_POINT('Ctrl Pts',(35.2766259050606,-71.984497206298,-26.9995817768601));
#27167=CARTESIAN_POINT('Ctrl Pts',(35.2806487513006,-71.9863593514082,-26.9995365071789));
#27168=CARTESIAN_POINT('Ctrl Pts',(35.2845900895339,-71.9881837792468,-26.9994888753932));
#27169=CARTESIAN_POINT('Ctrl Pts',(35.2882783929648,-71.9898910784073,-26.9994443015788));
#27170=CARTESIAN_POINT('Ctrl Pts',(35.2918949473981,-71.9915651760262,-26.9993976862506));
#27171=CARTESIAN_POINT('Ctrl Pts',(35.2954515321382,-71.993211531325,-26.9993491843894));
#27172=CARTESIAN_POINT('Ctrl Pts',(35.2990489039404,-71.994876767095,-26.9993001263068));
#27173=CARTESIAN_POINT('Ctrl Pts',(35.3025840722509,-71.9965132267008,-26.9992491748665));
#27174=CARTESIAN_POINT('Ctrl Pts',(35.3061197298406,-71.9981499419665,-26.9991955682734));
#27175=CARTESIAN_POINT('Ctrl Pts',(35.3095686516303,-71.999746505774,-26.9991432767429));
#27176=CARTESIAN_POINT('Ctrl Pts',(35.313026689874,-72.0013473181754,-26.9990883234737));
#27177=CARTESIAN_POINT('Ctrl Pts',(35.3165464873944,-72.0029767588717,-26.999029712487));
#27178=CARTESIAN_POINT('Ctrl Pts',(35.3202728437031,-72.0047018230503,-26.9989676619234));
#27179=CARTESIAN_POINT('Ctrl Pts',(35.3240680871851,-72.006458819974,-26.9989014928217));
#27180=CARTESIAN_POINT('Ctrl Pts',(35.3279399692184,-72.0082513459315,-26.9988307140748));
#27181=CARTESIAN_POINT('Ctrl Pts',(35.3321305670788,-72.010191424523,-26.9987541091413));
#27182=CARTESIAN_POINT('Ctrl Pts',(35.3364104437453,-72.0121728926466,-26.9986720801898));
#27183=CARTESIAN_POINT('Ctrl Pts',(35.3407333634553,-72.0141743492423,-26.9985851513296));
#27184=CARTESIAN_POINT('Ctrl Pts',(35.3457888070745,-72.0165149550492,-26.9984834922701));
#27185=CARTESIAN_POINT('Ctrl Pts',(35.3509023169183,-72.0188825276478,-26.9983750851363));
#27186=CARTESIAN_POINT('Ctrl Pts',(35.3559351026816,-72.0212128042074,-26.9982629447422));
#27187=CARTESIAN_POINT('Ctrl Pts',(35.3632986629101,-72.0246222741515,-26.9980988700955));
#27188=CARTESIAN_POINT('Ctrl Pts',(35.3704818772113,-72.0279484172625,-26.9979266950892));
#27189=CARTESIAN_POINT('Ctrl Pts',(35.3769682776864,-72.0309520300502,-26.9977626587855));
#27190=CARTESIAN_POINT('Ctrl Pts',(35.3811109071277,-72.0328703289298,-26.9976578947298));
#27191=CARTESIAN_POINT('Ctrl Pts',(35.3849676793297,-72.0346563122552,-26.9975566436896));
#27192=CARTESIAN_POINT('Ctrl Pts',(35.3884339927027,-72.0362615170312,-26.9974632996818));
#27193=CARTESIAN_POINT('Ctrl Pts',(35.3916379986998,-72.0377452506627,-26.9973770193232));
#27194=CARTESIAN_POINT('Ctrl Pts',(35.3945074173725,-72.0390740730493,-26.9972975574334));
#27195=CARTESIAN_POINT('Ctrl Pts',(35.3970049626025,-72.0402306971659,-26.9972272397508));
#27196=CARTESIAN_POINT('Ctrl Pts',(35.3991850734024,-72.0412403160099,-26.9971658593451));
#27197=CARTESIAN_POINT('Ctrl Pts',(35.4010819183648,-72.0421187666732,-26.9971114553097));
#27198=CARTESIAN_POINT('Ctrl Pts',(35.4027109342665,-72.0428731874732,-26.9970642613262));
#27199=CARTESIAN_POINT('Ctrl Pts',(35.404276671081,-72.0435983028137,-26.997018900592));
#27200=CARTESIAN_POINT('Ctrl Pts',(35.4055946392623,-72.0442086780501,-26.9969802139163));
#27201=CARTESIAN_POINT('Ctrl Pts',(35.4067209262391,-72.0447302826942,-26.9969469383907));
#27202=CARTESIAN_POINT('Ctrl Pts',(35.4077941440434,-72.0452273100082,-26.9969152307644));
#27203=CARTESIAN_POINT('Ctrl Pts',(35.40869316907,-72.0456436658995,-26.9968884389805));
#27204=CARTESIAN_POINT('Ctrl Pts',(35.4095091096287,-72.0460215435592,-26.9968640070379));
#27205=CARTESIAN_POINT('Ctrl Pts',(35.4100078256831,-72.0462525084911,-26.9968490738398));
#27206=CARTESIAN_POINT('Ctrl Pts',(35.4104763443426,-72.0464694884255,-26.9968349935969));
#27207=CARTESIAN_POINT('Ctrl Pts',(35.4109442661894,-72.0466861925664,-26.9968208864142));
#27208=CARTESIAN_POINT('Origin',(42.2,-32.,-20.));
#27209=CARTESIAN_POINT('',(42.2,-71.9490268349807,20.));
#27210=CARTESIAN_POINT('',(42.2,-32.,20.));
#27211=CARTESIAN_POINT('',(42.2,-72.5,18.8097619285762));
#27212=CARTESIAN_POINT('',(42.2,-72.2245134174903,19.4048809642881));
#27213=CARTESIAN_POINT('',(42.2,-72.5,-18.8097619285762));
#27214=CARTESIAN_POINT('',(42.2,-72.5,-10.));
#27215=CARTESIAN_POINT('',(42.2,-72.2245134174903,-19.4048809642881));
#27216=CARTESIAN_POINT('Origin',(35.2,-32.,20.));
#27217=CARTESIAN_POINT('',(35.2,-71.9490268349807,27.));
#27218=CARTESIAN_POINT('',(35.2,-32.,27.));
#27219=CARTESIAN_POINT('',(35.4109431177646,-72.046685660721,26.9968209210375));
#27220=CARTESIAN_POINT('Ctrl Pts',(35.4109431177646,-72.046685660721,26.9968209210375));
#27221=CARTESIAN_POINT('Ctrl Pts',(35.4101765648703,-72.0463306544709,26.9968440313985));
#27222=CARTESIAN_POINT('Ctrl Pts',(35.4094058110184,-72.0459737040598,26.9968671567182));
#27223=CARTESIAN_POINT('Ctrl Pts',(35.4085104131101,-72.0455590281861,26.9968938399567));
#27224=CARTESIAN_POINT('Ctrl Pts',(35.407579559468,-72.0451279320849,26.9969215797913));
#27225=CARTESIAN_POINT('Ctrl Pts',(35.406514196614,-72.0446345417411,26.9969531606685));
#27226=CARTESIAN_POINT('Ctrl Pts',(35.4052317858403,-72.0440406347175,26.9969907756178));
#27227=CARTESIAN_POINT('Ctrl Pts',(35.4038863137786,-72.0434175229004,26.9970302402452));
#27228=CARTESIAN_POINT('Ctrl Pts',(35.4023021774198,-72.0426838837104,26.9970763400508));
#27229=CARTESIAN_POINT('Ctrl Pts',(35.4004376036754,-72.0418203796692,26.9971297520507));
#27230=CARTESIAN_POINT('Ctrl Pts',(35.398452200092,-72.0409009180375,26.9971866253045));
#27231=CARTESIAN_POINT('Ctrl Pts',(35.3961491809414,-72.0398343752723,26.9972517711657));
#27232=CARTESIAN_POINT('Ctrl Pts',(35.3935328802145,-72.0386227730735,26.9973241331437));
#27233=CARTESIAN_POINT('Ctrl Pts',(35.3906684528407,-72.0372962640568,26.9974033578401));
#27234=CARTESIAN_POINT('Ctrl Pts',(35.3874290419011,-72.0357961260639,26.9974911916518));
#27235=CARTESIAN_POINT('Ctrl Pts',(35.3838773827663,-72.0341514325885,26.9975845195401));
#27236=CARTESIAN_POINT('Ctrl Pts',(35.379506277065,-72.0321272718359,26.9976993802429));
#27237=CARTESIAN_POINT('Ctrl Pts',(35.3746631927677,-72.0298846097018,26.9978224504091));
#27238=CARTESIAN_POINT('Ctrl Pts',(35.3695384544159,-72.02751161209,26.9979466068608));
#27239=CARTESIAN_POINT('Ctrl Pts',(35.3639434120815,-72.0249208413645,26.9980821573134));
#27240=CARTESIAN_POINT('Ctrl Pts',(35.3580183169952,-72.0221773413901,26.998218776321));
#27241=CARTESIAN_POINT('Ctrl Pts',(35.3520339326916,-72.0194065054176,26.998348782628));
#27242=CARTESIAN_POINT('Ctrl Pts',(35.3474966654497,-72.0173057006142,26.998447351391));
#27243=CARTESIAN_POINT('Ctrl Pts',(35.3429265908979,-72.0151897711979,26.998542158666));
#27244=CARTESIAN_POINT('Ctrl Pts',(35.3384155986028,-72.0131012617228,26.9986313749235));
#27245=CARTESIAN_POINT('Ctrl Pts',(35.3343447547669,-72.0112165331826,26.9987118861344));
#27246=CARTESIAN_POINT('Ctrl Pts',(35.3303225957582,-72.0093543982207,26.9987878633368));
#27247=CARTESIAN_POINT('Ctrl Pts',(35.326381797399,-72.0075299799367,26.9988590242472));
#27248=CARTESIAN_POINT('Ctrl Pts',(35.3226939903455,-72.0058226856266,26.9989256167707));
#27249=CARTESIAN_POINT('Ctrl Pts',(35.3190778042077,-72.0041485925122,26.99898800739));
#27250=CARTESIAN_POINT('Ctrl Pts',(35.3155214580876,-72.0025022394492,26.9990467059966));
#27251=CARTESIAN_POINT('Ctrl Pts',(35.3119233667752,-72.0008365611229,26.9991060936207));
#27252=CARTESIAN_POINT('Ctrl Pts',(35.3083873825375,-71.9991996731568,26.9991617130831));
#27253=CARTESIAN_POINT('Ctrl Pts',(35.3048507493789,-71.9975625131321,26.9992146931177));
#27254=CARTESIAN_POINT('Ctrl Pts',(35.3014017990027,-71.9959659427698,26.9992663596328));
#27255=CARTESIAN_POINT('Ctrl Pts',(35.2979435804289,-71.9943651083224,26.9993156414398));
#27256=CARTESIAN_POINT('Ctrl Pts',(35.2944234673532,-71.9927356391638,26.9993631288006));
#27257=CARTESIAN_POINT('Ctrl Pts',(35.2906967521995,-71.9910105333859,26.9994134032842));
#27258=CARTESIAN_POINT('Ctrl Pts',(35.2869009967207,-71.9892534872448,26.9994616375389));
#27259=CARTESIAN_POINT('Ctrl Pts',(35.2830284653437,-71.9874609128098,26.9995075736756));
#27260=CARTESIAN_POINT('Ctrl Pts',(35.2788371112672,-71.9855207570216,26.9995572917012));
#27261=CARTESIAN_POINT('Ctrl Pts',(35.2745563143599,-71.9835392115203,26.9996042784301));
#27262=CARTESIAN_POINT('Ctrl Pts',(35.2702323409792,-71.9815376862603,26.9996476638671));
#27263=CARTESIAN_POINT('Ctrl Pts',(35.2651754999054,-71.9791969236667,26.9996984026762));
#27264=CARTESIAN_POINT('Ctrl Pts',(35.2600604049209,-71.9768292045288,26.9997441449775));
#27265=CARTESIAN_POINT('Ctrl Pts',(35.2550259417389,-71.9744988084769,26.9997837213542));
#27266=CARTESIAN_POINT('Ctrl Pts',(35.2476608969128,-71.9710896125479,26.999841618647));
#27267=CARTESIAN_POINT('Ctrl Pts',(35.2404759526217,-71.9677637815365,26.9998859843948));
#27268=CARTESIAN_POINT('Ctrl Pts',(35.2339877884408,-71.9647604551991,26.9999174873878));
#27269=CARTESIAN_POINT('Ctrl Pts',(35.2298440288371,-71.9628423375302,26.9999376072285));
#27270=CARTESIAN_POINT('Ctrl Pts',(35.225986116163,-71.9610565242505,26.9999526244651));
#27271=CARTESIAN_POINT('Ctrl Pts',(35.2225187158526,-71.9594514605142,26.9999637790089));
#27272=CARTESIAN_POINT('Ctrl Pts',(35.2193137088523,-71.9579678589538,26.9999740894397));
#27273=CARTESIAN_POINT('Ctrl Pts',(35.2164433351698,-71.9566391432609,26.9999811327487));
#27274=CARTESIAN_POINT('Ctrl Pts',(35.2139449186996,-71.9554825904979,26.9999861099321));
#27275=CARTESIAN_POINT('Ctrl Pts',(35.211763953714,-71.9544729905733,26.9999904547092));
#27276=CARTESIAN_POINT('Ctrl Pts',(35.209866343227,-71.9535945432724,26.9999932365079));
#27277=CARTESIAN_POINT('Ctrl Pts',(35.2082366558696,-71.9528401072575,26.9999951541055));
#27278=CARTESIAN_POINT('Ctrl Pts',(35.2066702690583,-71.9521149751525,26.9999969972195));
#27279=CARTESIAN_POINT('Ctrl Pts',(35.2053517394672,-71.9515045666398,26.9999980448942));
#27280=CARTESIAN_POINT('Ctrl Pts',(35.2042249574883,-71.9509829115285,26.9999987249809));
#27281=CARTESIAN_POINT('Ctrl Pts',(35.2031512632312,-71.9504858339147,26.9999993730257));
#27282=CARTESIAN_POINT('Ctrl Pts',(35.2022518236115,-71.9500694128274,26.9999996854072));
#27283=CARTESIAN_POINT('Ctrl Pts',(35.2014354838484,-71.9496914561438,26.9999998528133));
#27284=CARTESIAN_POINT('Ctrl Pts',(35.2009366676327,-71.9494605095072,26.9999999551051));
#27285=CARTESIAN_POINT('Ctrl Pts',(35.2004680362892,-71.9492435345226,27.));
#27286=CARTESIAN_POINT('Ctrl Pts',(35.2,-71.9490268349807,27.));
#27287=CARTESIAN_POINT('',(39.0078632855922,-73.4473505180018,25.8736851463318));
#27288=CARTESIAN_POINT('Ctrl Pts',(39.0078632855927,-73.4473505180019,25.8736851463315));
#27289=CARTESIAN_POINT('Ctrl Pts',(38.7006130536539,-73.3910116765338,26.0728730238806));
#27290=CARTESIAN_POINT('Ctrl Pts',(38.1887966829792,-73.2378094420153,26.3429260072132));
#27291=CARTESIAN_POINT('Ctrl Pts',(37.0808170189174,-72.8203441337222,26.7897806502721));
#27292=CARTESIAN_POINT('Ctrl Pts',(36.0964746307403,-72.3641692597616,26.9761532269083));
#27293=CARTESIAN_POINT('Ctrl Pts',(35.4109431177646,-72.046685660721,26.9968209210375));
#27294=CARTESIAN_POINT('',(39.5301270189222,-73.5,25.5));
#27295=CARTESIAN_POINT('Ctrl Pts',(39.5301270189222,-73.5,25.5));
#27296=CARTESIAN_POINT('Ctrl Pts',(39.3719134220716,-73.5,25.6245609037243));
#27297=CARTESIAN_POINT('Ctrl Pts',(39.195551811226,-73.4817659650606,25.75200817045));
#27298=CARTESIAN_POINT('Ctrl Pts',(39.0078632855922,-73.4473505180018,25.8736851463318));
#27299=CARTESIAN_POINT('',(40.7,-73.5,24.3301270189222));
#27300=CARTESIAN_POINT('Origin',(35.2,-73.5,20.));
#27301=CARTESIAN_POINT('',(41.0736851473658,-73.4473505177094,23.8078632839972));
#27302=CARTESIAN_POINT('Ctrl Pts',(41.0736851473658,-73.4473505177094,23.8078632839972));
#27303=CARTESIAN_POINT('Ctrl Pts',(40.9547480121633,-73.4809910208687,23.9913255651787));
#27304=CARTESIAN_POINT('Ctrl Pts',(40.8292080416589,-73.5,24.1660107641291));
#27305=CARTESIAN_POINT('Ctrl Pts',(40.7,-73.5,24.3301270189222));
#27306=CARTESIAN_POINT('',(42.196820839876,-72.0466869074717,20.2109458098101));
#27307=CARTESIAN_POINT('Ctrl Pts',(42.196820839876,-72.0466869074717,20.2109458098101));
#27308=CARTESIAN_POINT('Ctrl Pts',(42.1783550388962,-72.3303428376334,20.8234343974591));
#27309=CARTESIAN_POINT('Ctrl Pts',(41.9708816473713,-72.9316905412085,22.1114797855899));
#27310=CARTESIAN_POINT('Ctrl Pts',(41.409110668669,-73.3524778499768,23.2904644816805));
#27311=CARTESIAN_POINT('Ctrl Pts',(41.0736851473658,-73.4473505177094,23.8078632839972));
#27312=CARTESIAN_POINT('Ctrl Pts',(42.2,-71.9490268349807,20.));
#27313=CARTESIAN_POINT('Ctrl Pts',(42.2,-71.9493819426082,20.0007669743775));
#27314=CARTESIAN_POINT('Ctrl Pts',(42.199999888335,-71.9497389941748,20.0015381483622));
#27315=CARTESIAN_POINT('Ctrl Pts',(42.199999576824,-71.9501537653895,20.0024340223005));
#27316=CARTESIAN_POINT('Ctrl Pts',(42.1999992529782,-71.9505849600876,20.0033653697007));
#27317=CARTESIAN_POINT('Ctrl Pts',(42.1999987149955,-71.9510784426047,20.0044312863678));
#27318=CARTESIAN_POINT('Ctrl Pts',(42.1999976675908,-71.9516724317248,20.0057143436616));
#27319=CARTESIAN_POINT('Ctrl Pts',(42.199996568683,-71.9522956285314,20.0070604915641));
#27320=CARTESIAN_POINT('Ctrl Pts',(42.1999949097774,-71.9530293412267,20.0086454048492));
#27321=CARTESIAN_POINT('Ctrl Pts',(42.1999921086958,-71.9538929058103,20.0105108608933));
#27322=CARTESIAN_POINT('Ctrl Pts',(42.1999891261053,-71.954812429029,20.012497197733));
#27323=CARTESIAN_POINT('Ctrl Pts',(42.1999848409495,-71.9558790177824,20.0148012672521));
#27324=CARTESIAN_POINT('Ctrl Pts',(42.1999783277262,-71.9570906515628,20.0174187072715));
#27325=CARTESIAN_POINT('Ctrl Pts',(42.1999711968435,-71.9584171865341,20.0202843633612));
#27326=CARTESIAN_POINT('Ctrl Pts',(42.1999613708697,-71.9599173309903,20.0235251037887));
#27327=CARTESIAN_POINT('Ctrl Pts',(42.1999476265851,-71.9615620166934,20.027078128906));
#27328=CARTESIAN_POINT('Ctrl Pts',(42.1999307119774,-71.9635860735613,20.0314507119941));
#27329=CARTESIAN_POINT('Ctrl Pts',(42.1999077801504,-71.9658285899073,20.0362952820845));
#27330=CARTESIAN_POINT('Ctrl Pts',(42.1998774465528,-71.9682014260206,20.0414214104202));
#27331=CARTESIAN_POINT('Ctrl Pts',(42.1998443239922,-71.9707924278841,20.0470188505451));
#27332=CARTESIAN_POINT('Ctrl Pts',(42.1998023205894,-71.9735361891088,20.0529463298847));
#27333=CARTESIAN_POINT('Ctrl Pts',(42.1997519182532,-71.9763072902013,20.0589328678251));
#27334=CARTESIAN_POINT('Ctrl Pts',(42.1997137069337,-71.9784081338789,20.0634714176514));
#27335=CARTESIAN_POINT('Ctrl Pts',(42.199670746498,-71.9805241019789,20.0680426384819));
#27336=CARTESIAN_POINT('Ctrl Pts',(42.1996239777039,-71.9826126499435,20.0725546053147));
#27337=CARTESIAN_POINT('Ctrl Pts',(42.1995817725225,-71.9844974012468,20.0766263027394));
#27338=CARTESIAN_POINT('Ctrl Pts',(42.1995365022911,-71.9863595591176,20.0806491768695));
#27339=CARTESIAN_POINT('Ctrl Pts',(42.1994888699131,-71.9881839996438,20.0845905429849));
#27340=CARTESIAN_POINT('Ctrl Pts',(42.1994442955512,-71.9898913104193,20.0882788719507));
#27341=CARTESIAN_POINT('Ctrl Pts',(42.1993976796393,-71.9915654195986,20.0918954519325));
#27342=CARTESIAN_POINT('Ctrl Pts',(42.1993491771674,-71.9932117861756,20.0954520617162));
#27343=CARTESIAN_POINT('Ctrl Pts',(42.1993001195776,-71.9948769956621,20.0990493774263));
#27344=CARTESIAN_POINT('Ctrl Pts',(42.1992491686837,-71.9965134300916,20.1025844921456));
#27345=CARTESIAN_POINT('Ctrl Pts',(42.1991955627639,-71.9981501187984,20.106120093224));
#27346=CARTESIAN_POINT('Ctrl Pts',(42.1991432708539,-71.9997466883352,20.1095690282307));
#27347=CARTESIAN_POINT('Ctrl Pts',(42.1990883172282,-72.0013475051531,20.1130270769141));
#27348=CARTESIAN_POINT('Ctrl Pts',(42.1990297058862,-72.0029769497589,20.1165468837949));
#27349=CARTESIAN_POINT('Ctrl Pts',(42.198967654991,-72.0047020168383,20.1202732473384));
#27350=CARTESIAN_POINT('Ctrl Pts',(42.1989014855651,-72.0064590160509,20.1240684967513));
#27351=CARTESIAN_POINT('Ctrl Pts',(42.1988307064682,-72.0082515445906,20.1279403853283));
#27352=CARTESIAN_POINT('Ctrl Pts',(42.1987541012615,-72.0101916233066,20.1321309845027));
#27353=CARTESIAN_POINT('Ctrl Pts',(42.1986720720218,-72.0121730917887,20.136410862965));
#27354=CARTESIAN_POINT('Ctrl Pts',(42.1985851428042,-72.0141745501329,20.1407337874152));
#27355=CARTESIAN_POINT('Ctrl Pts',(42.198483483764,-72.0165151479206,20.1457892148409));
#27356=CARTESIAN_POINT('Ctrl Pts',(42.1983750766135,-72.0188827141844,20.1509027120514));
#27357=CARTESIAN_POINT('Ctrl Pts',(42.198262936023,-72.021212988539,20.1559354939934));
#27358=CARTESIAN_POINT('Ctrl Pts',(42.1980988580267,-72.0246225188898,20.1632991860607));
#27359=CARTESIAN_POINT('Ctrl Pts',(42.1979266789503,-72.0279487284441,20.17048254499));
#27360=CARTESIAN_POINT('Ctrl Pts',(42.1977626383687,-72.0309524054426,20.1769690850139));
#27361=CARTESIAN_POINT('Ctrl Pts',(42.1976578720763,-72.0328707362592,20.1811117839881));
#27362=CARTESIAN_POINT('Ctrl Pts',(42.1975566186956,-72.0346567517583,20.1849686261325));
#27363=CARTESIAN_POINT('Ctrl Pts',(42.1974632723898,-72.0362619872375,20.1884350061837));
#27364=CARTESIAN_POINT('Ctrl Pts',(42.1973769893887,-72.0377457581639,20.1916390930644));
#27365=CARTESIAN_POINT('Ctrl Pts',(42.1972975249792,-72.0390746146824,20.1945085857143));
#27366=CARTESIAN_POINT('Ctrl Pts',(42.1972272050586,-72.040231268269,20.1970061947958));
#27367=CARTESIAN_POINT('Ctrl Pts',(42.1971658233327,-72.0412409024212,20.1991863388396));
#27368=CARTESIAN_POINT('Ctrl Pts',(42.1971114180469,-72.0421193675758,20.2010832152381));
#27369=CARTESIAN_POINT('Ctrl Pts',(42.1970642229353,-72.0428738014203,20.2027122594201));
#27370=CARTESIAN_POINT('Ctrl Pts',(42.197018861125,-72.043598929167,20.2042780231325));
#27371=CARTESIAN_POINT('Ctrl Pts',(42.1969801734843,-72.0442093155135,20.2055960153841));
#27372=CARTESIAN_POINT('Ctrl Pts',(42.1969468971449,-72.0447309293597,20.2067223222945));
#27373=CARTESIAN_POINT('Ctrl Pts',(42.1969151887602,-72.0452279651743,20.2077955585147));
#27374=CARTESIAN_POINT('Ctrl Pts',(42.1968883963498,-72.0456443279215,20.2086945983907));
#27375=CARTESIAN_POINT('Ctrl Pts',(42.1968639639419,-72.0460222101615,20.2095105488797));
#27376=CARTESIAN_POINT('Ctrl Pts',(42.1968490294804,-72.0462531930326,20.2100093036948));
#27377=CARTESIAN_POINT('Ctrl Pts',(42.1968349481487,-72.0464701881852,20.2104778552371));
#27378=CARTESIAN_POINT('Ctrl Pts',(42.196820839876,-72.0466869074717,20.2109458098101));
#27379=CARTESIAN_POINT('Ctrl Pts',(-4.59286786251854,-72.9498130615488,
-26.9309675781303));
#27380=CARTESIAN_POINT('Ctrl Pts',(-4.58597883112302,-72.9467708226897,
-26.9319238812612));
#27381=CARTESIAN_POINT('Ctrl Pts',(-4.57152330186566,-72.9403541543873,
-26.9337973859128));
#27382=CARTESIAN_POINT('Ctrl Pts',(-4.48780388137234,-72.9035146304749,
-26.9456499185224));
#27383=CARTESIAN_POINT('Ctrl Pts',(-4.23649589071421,-72.7907458248883,
-26.9734457827405));
#27384=CARTESIAN_POINT('Ctrl Pts',(-3.96644514618002,-72.665579126758,-26.9924939495254));
#27385=CARTESIAN_POINT('Ctrl Pts',(-3.71514557682102,-72.548594622924,-27.0001369004246));
#27386=CARTESIAN_POINT('Ctrl Pts',(-3.63119107772806,-72.5097909109609,
-26.9998430869986));
#27387=CARTESIAN_POINT('Ctrl Pts',(-3.61668235972474,-72.5031611812015,
-27.));
#27388=CARTESIAN_POINT('Ctrl Pts',(-3.60976192857618,-72.5,-27.));
#27389=CARTESIAN_POINT('Ctrl Pts',(-4.73222628093364,-72.6487705946061,
-26.9529186924327));
#27390=CARTESIAN_POINT('Ctrl Pts',(-4.72712574225606,-72.6464928862309,
-26.9533741257428));
#27391=CARTESIAN_POINT('Ctrl Pts',(-4.71810316556283,-72.6424665759273,
-26.9541650696995));
#27392=CARTESIAN_POINT('Ctrl Pts',(-4.66022923522091,-72.6172314047933,
-26.9623845226138));
#27393=CARTESIAN_POINT('Ctrl Pts',(-4.46228371256307,-72.5287892895904,
-26.9851096971082));
#27394=CARTESIAN_POINT('Ctrl Pts',(-4.27646988143267,-72.442180089981,-26.9974869463342));
#27395=CARTESIAN_POINT('Ctrl Pts',(-4.07861559516288,-72.3497082397124,
-27.0015613961821));
#27396=CARTESIAN_POINT('Ctrl Pts',(-4.02063676120937,-72.3228011601093,
-26.9999955597789));
#27397=CARTESIAN_POINT('Ctrl Pts',(-4.01161227485084,-72.3186769260278,
-27.));
#27398=CARTESIAN_POINT('Ctrl Pts',(-4.00650795238412,-72.3163422783269,
-27.));
#27399=CARTESIAN_POINT('Ctrl Pts',(-4.87158469934875,-72.3477281276634,
-26.9748698067351));
#27400=CARTESIAN_POINT('Ctrl Pts',(-4.86830808893293,-72.346245599186,-26.9750197376998));
#27401=CARTESIAN_POINT('Ctrl Pts',(-4.85975975168661,-72.3423622412983,
-26.9755924149209));
#27402=CARTESIAN_POINT('Ctrl Pts',(-4.81588843551312,-72.3223172404505,
-26.9789296879549));
#27403=CARTESIAN_POINT('Ctrl Pts',(-4.70844366796589,-72.2729883046416,
-26.9857195731902));
#27404=CARTESIAN_POINT('Ctrl Pts',(-4.56627474372858,-72.2076842290428,
-26.9947091274986));
#27405=CARTESIAN_POINT('Ctrl Pts',(-4.45897436459025,-72.1582939535662,
-26.9983929926645));
#27406=CARTESIAN_POINT('Ctrl Pts',(-4.41510722369007,-72.138122645422,-26.999758423857));
#27407=CARTESIAN_POINT('Ctrl Pts',(-4.40654218997694,-72.1341926708542,
-27.));
#27408=CARTESIAN_POINT('Ctrl Pts',(-4.40325397619206,-72.1326845566538,
-27.));
#27409=CARTESIAN_POINT('Ctrl Pts',(-5.01094311776385,-72.0466856607207,
-26.9968209210375));
#27410=CARTESIAN_POINT('Ctrl Pts',(-5.00947183604093,-72.0460042802039,
-26.9968652778614));
#27411=CARTESIAN_POINT('Ctrl Pts',(-5.00638341486692,-72.0445740412427,
-26.9969519897208));
#27412=CARTESIAN_POINT('Ctrl Pts',(-4.98844404444095,-72.0362656438942,
-26.9975053631966));
#27413=CARTESIAN_POINT('Ctrl Pts',(-4.93447171373018,-72.0112738204271,
-26.9987930811475));
#27414=CARTESIAN_POINT('Ctrl Pts',(-4.87648104575523,-71.9844301094941,
-26.9996559735758));
#27415=CARTESIAN_POINT('Ctrl Pts',(-4.8225217894526,-71.959453134982,-27.0000061189091));
#27416=CARTESIAN_POINT('Ctrl Pts',(-4.80456005745059,-71.9511381192262,
-26.9999927847699));
#27417=CARTESIAN_POINT('Ctrl Pts',(-4.80147210510304,-71.9497084156806,
-27.));
#27418=CARTESIAN_POINT('Ctrl Pts',(-4.8,-71.9490268349807,-27.));
#27419=CARTESIAN_POINT('',(-4.59286786251854,-72.9498130615488,-26.9309675781303));
#27420=CARTESIAN_POINT('Ctrl Pts',(-3.60976192857618,-72.5,-27.));
#27421=CARTESIAN_POINT('Ctrl Pts',(-3.6121798317656,-72.5011044731095,-27.));
#27422=CARTESIAN_POINT('Ctrl Pts',(-3.61460175619875,-72.5022108180881,
-26.9999988447398));
#27423=CARTESIAN_POINT('Ctrl Pts',(-3.61720808063408,-72.5034032651581,
-26.9999961392571));
#27424=CARTESIAN_POINT('Ctrl Pts',(-3.61987818981872,-72.5046248950636,
-26.999993367563));
#27425=CARTESIAN_POINT('Ctrl Pts',(-3.62274171103015,-72.5059368360811,
-26.9999889713356));
#27426=CARTESIAN_POINT('Ctrl Pts',(-3.62594300170539,-72.5074065633977,
-26.9999817141614));
#27427=CARTESIAN_POINT('Ctrl Pts',(-3.6292333827049,-72.5089171924931,-26.9999742550237));
#27428=CARTESIAN_POINT('Ctrl Pts',(-3.63288045211659,-72.5105944472574,
-26.9999637812448));
#27429=CARTESIAN_POINT('Ctrl Pts',(-3.63699121203846,-72.5124884140809,
-26.9999480122703));
#27430=CARTESIAN_POINT('Ctrl Pts',(-3.64123459139212,-72.5144434831845,
-26.9999317345645));
#27431=CARTESIAN_POINT('Ctrl Pts',(-3.64597189527866,-72.5166293969509,
-26.9999098171331));
#27432=CARTESIAN_POINT('Ctrl Pts',(-3.65127087672114,-72.5190779485736,
-26.9998786723859));
#27433=CARTESIAN_POINT('Ctrl Pts',(-3.65689722795564,-72.5216777711234,
-26.9998456035239));
#27434=CARTESIAN_POINT('Ctrl Pts',(-3.66315677356868,-72.5245736760054,
-26.9998021229674));
#27435=CARTESIAN_POINT('Ctrl Pts',(-3.67007637899193,-72.5277783735898,
-26.9997427652637));
#27436=CARTESIAN_POINT('Ctrl Pts',(-3.67736092134016,-72.5311520855053,
-26.9996802770609));
#27437=CARTESIAN_POINT('Ctrl Pts',(-3.68537672523341,-72.5348679050117,
-26.9996001514933));
#27438=CARTESIAN_POINT('Ctrl Pts',(-3.69409908715974,-72.538914401124,-26.9994951381666));
#27439=CARTESIAN_POINT('Ctrl Pts',(-3.70344137655423,-72.5432484952644,
-26.9993826611911));
#27440=CARTESIAN_POINT('Ctrl Pts',(-3.71359387467642,-72.5479617814959,
-26.9992415459466));
#27441=CARTESIAN_POINT('Ctrl Pts',(-3.7244680994068,-72.5530128872099,-26.999062918556));
#27442=CARTESIAN_POINT('Ctrl Pts',(-3.7365221810632,-72.5586120395395,-26.9988649100353));
#27443=CARTESIAN_POINT('Ctrl Pts',(-3.74946252996333,-72.5646260341567,
-26.9986206326566));
#27444=CARTESIAN_POINT('Ctrl Pts',(-3.76310633289472,-72.5709691128928,
-26.9983201877487));
#27445=CARTESIAN_POINT('Ctrl Pts',(-3.77980856865807,-72.5787340738093,
-26.9979523942741));
#27446=CARTESIAN_POINT('Ctrl Pts',(-3.79756346992481,-72.5869914895461,
-26.9974999166189));
#27447=CARTESIAN_POINT('Ctrl Pts',(-3.815960640567,-72.5955484292695,-26.99695373932));
#27448=CARTESIAN_POINT('Ctrl Pts',(-3.83486113114969,-72.604339474469,-26.9963926194013));
#27449=CARTESIAN_POINT('Ctrl Pts',(-3.85443398804955,-72.6134440505967,
-26.9957325028426));
#27450=CARTESIAN_POINT('Ctrl Pts',(-3.87422314146776,-72.6226474512837,
-26.9949774589249));
#27451=CARTESIAN_POINT('Ctrl Pts',(-3.89002366524084,-72.6299958480683,
-26.9943745989077));
#27452=CARTESIAN_POINT('Ctrl Pts',(-3.90596073606572,-72.6374066137615,
-26.9937116122647));
#27453=CARTESIAN_POINT('Ctrl Pts',(-3.92183420187478,-72.644785372869,-26.9929960468143));
#27454=CARTESIAN_POINT('Ctrl Pts',(-3.93600161067149,-72.6513710736823,
-26.9923573892975));
#27455=CARTESIAN_POINT('Ctrl Pts',(-3.95011786238888,-72.6579310555987,
-26.9916770268006));
#27456=CARTESIAN_POINT('Ctrl Pts',(-3.96407960253109,-72.6644163574739,
-26.9909618577935));
#27457=CARTESIAN_POINT('Ctrl Pts',(-3.97708743249592,-72.6704585630446,
-26.9902955513915));
#27458=CARTESIAN_POINT('Ctrl Pts',(-3.98996081458732,-72.676435800597,-26.9895991550418));
#27459=CARTESIAN_POINT('Ctrl Pts',(-4.00265755428967,-72.6823276467238,
-26.9888776407886));
#27460=CARTESIAN_POINT('Ctrl Pts',(-4.01471371198153,-72.6879222345996,
-26.988192528719));
#27461=CARTESIAN_POINT('Ctrl Pts',(-4.02661035498069,-72.6934397254355,
-26.9874848652863));
#27462=CARTESIAN_POINT('Ctrl Pts',(-4.03835411814552,-72.6988823143548,
-26.986756814357));
#27463=CARTESIAN_POINT('Ctrl Pts',(-4.0496271379236,-72.7041067395813,-26.9860579470169));
#27464=CARTESIAN_POINT('Ctrl Pts',(-4.06075909094922,-72.7092620662293,
-26.9853403733249));
#27465=CARTESIAN_POINT('Ctrl Pts',(-4.07179949547093,-72.7143701921724,
-26.9846027821299));
#27466=CARTESIAN_POINT('Ctrl Pts',(-4.08305161322444,-72.7195762726651,
-26.9838510467236));
#27467=CARTESIAN_POINT('Ctrl Pts',(-4.09420802299186,-72.7247330573131,
-26.9830786440317));
#27468=CARTESIAN_POINT('Ctrl Pts',(-4.10537436234696,-72.729887888526,-26.9822791770477));
#27469=CARTESIAN_POINT('Ctrl Pts',(-4.11610685214918,-72.7348424373415,
-26.9815107720242));
#27470=CARTESIAN_POINT('Ctrl Pts',(-4.12685642878814,-72.7397987793188,
-26.9807167793448));
#27471=CARTESIAN_POINT('Ctrl Pts',(-4.13770638415419,-72.7447940225878,
-26.9798904981468));
#27472=CARTESIAN_POINT('Ctrl Pts',(-4.14894230031643,-72.7499669594974,
-26.9790348240032));
#27473=CARTESIAN_POINT('Ctrl Pts',(-4.16028567191421,-72.755181518857,-26.9781444707583));
#27474=CARTESIAN_POINT('Ctrl Pts',(-4.17177856524463,-72.7604559078795,
-26.9772145138912));
#27475=CARTESIAN_POINT('Ctrl Pts',(-4.1840671780142,-72.7660954733422,-26.9762201707346));
#27476=CARTESIAN_POINT('Ctrl Pts',(-4.19652668861544,-72.771803406091,-26.9751804717657));
#27477=CARTESIAN_POINT('Ctrl Pts',(-4.20915332155542,-72.7775769562583,
-26.974093291944));
#27478=CARTESIAN_POINT('Ctrl Pts',(-4.2225448421669,-72.7837002526615,-26.9729402536749));
#27479=CARTESIAN_POINT('Ctrl Pts',(-4.23612401933091,-72.7898971879111,
-26.9717337257237));
#27480=CARTESIAN_POINT('Ctrl Pts',(-4.24982926006434,-72.7961388946508,
-26.9704767101437));
#27481=CARTESIAN_POINT('Ctrl Pts',(-4.26471116374373,-72.8029164828962,
-26.9691117735367));
#27482=CARTESIAN_POINT('Ctrl Pts',(-4.27974121837608,-72.809746603987,-26.967687199763));
#27483=CARTESIAN_POINT('Ctrl Pts',(-4.2947812708956,-72.8165662126102,-26.9662147977134));
#27484=CARTESIAN_POINT('Ctrl Pts',(-4.31217847082007,-72.8244546222066,
-26.964511633925));
#27485=CARTESIAN_POINT('Ctrl Pts',(-4.32958814165081,-72.8323284779439,
-26.9627442813405));
#27486=CARTESIAN_POINT('Ctrl Pts',(-4.34673013421309,-72.8400621253335,
-26.9609441299768));
#27487=CARTESIAN_POINT('Ctrl Pts',(-4.36908646666351,-72.8501482335539,
-26.958596399268));
#27488=CARTESIAN_POINT('Ctrl Pts',(-4.3909822100646,-72.8599932152661,-26.9561926445271));
#27489=CARTESIAN_POINT('Ctrl Pts',(-4.41173359126681,-72.8692963615835,
-26.9538294938958));
#27490=CARTESIAN_POINT('Ctrl Pts',(-4.42638773343343,-72.87586602687,-26.9521606919508));
#27491=CARTESIAN_POINT('Ctrl Pts',(-4.44046920811496,-72.882164767821,-26.9505129508519));
#27492=CARTESIAN_POINT('Ctrl Pts',(-4.45375849835115,-72.8880981139709,
-26.9489236880982));
#27493=CARTESIAN_POINT('Ctrl Pts',(-4.46568249135964,-72.8934218879838,
-26.947497700884));
#27494=CARTESIAN_POINT('Ctrl Pts',(-4.47696801229591,-72.8984512256794,
-26.9461190319865));
#27495=CARTESIAN_POINT('Ctrl Pts',(-4.4874906704524,-72.9031338368651,-26.9448124824954));
#27496=CARTESIAN_POINT('Ctrl Pts',(-4.49731427885776,-72.9075053690311,
-26.9435927307584));
#27497=CARTESIAN_POINT('Ctrl Pts',(-4.50647257936972,-72.9115745492459,
-26.9424359792803));
#27498=CARTESIAN_POINT('Ctrl Pts',(-4.51490348064674,-72.9153163971461,
-26.9413577939781));
#27499=CARTESIAN_POINT('Ctrl Pts',(-4.52291802255619,-72.918873454195,-26.9403328547686));
#27500=CARTESIAN_POINT('Ctrl Pts',(-4.53027491933034,-72.9221345908914,
-26.939379007774));
#27501=CARTESIAN_POINT('Ctrl Pts',(-4.53696273809178,-72.9250967827365,
-26.9385036410476));
#27502=CARTESIAN_POINT('Ctrl Pts',(-4.54338726026832,-72.9279423543464,
-26.9376627371375));
#27503=CARTESIAN_POINT('Ctrl Pts',(-4.54919410148017,-72.9305119583038,
-26.9368943156625));
#27504=CARTESIAN_POINT('Ctrl Pts',(-4.55441685885851,-72.932821936876,-26.93619816563));
#27505=CARTESIAN_POINT('Ctrl Pts',(-4.55939180148987,-72.9350223092165,
-26.9355350472379));
#27506=CARTESIAN_POINT('Ctrl Pts',(-4.56383669313756,-72.9369870780139,
-26.9349375205309));
#27507=CARTESIAN_POINT('Ctrl Pts',(-4.56782323678299,-72.9387488347678,
-26.9343986405424));
#27508=CARTESIAN_POINT('Ctrl Pts',(-4.5717196612956,-72.9404707655458,-26.933871942384));
#27509=CARTESIAN_POINT('Ctrl Pts',(-4.57517802327509,-72.9419986707184,
-26.9334012948219));
#27510=CARTESIAN_POINT('Ctrl Pts',(-4.57830933875514,-72.9433820368179,
-26.9329732619373));
#27511=CARTESIAN_POINT('Ctrl Pts',(-4.58134224987413,-72.9447219294131,
-26.932558680365));
#27512=CARTESIAN_POINT('Ctrl Pts',(-4.58406826147243,-72.9459261859508,
-26.9321840818725));
#27513=CARTESIAN_POINT('Ctrl Pts',(-4.58663203070186,-72.9470587250243,
-26.9318304705445));
#27514=CARTESIAN_POINT('Ctrl Pts',(-4.58878734423874,-72.9480108297488,
-26.9315331960186));
#27515=CARTESIAN_POINT('Ctrl Pts',(-4.59082864516527,-72.9489125305571,
-26.9312506527496));
#27516=CARTESIAN_POINT('Ctrl Pts',(-4.59286786251854,-72.9498130615488,
-26.9309675781303));
#27517=CARTESIAN_POINT('',(-5.01094311776385,-72.0466856607207,-26.9968209210375));
#27518=CARTESIAN_POINT('Ctrl Pts',(-5.01094311776385,-72.0466856607207,
-26.9968209210375));
#27519=CARTESIAN_POINT('Ctrl Pts',(-4.87158469934875,-72.3477281276634,
-26.9748698067351));
#27520=CARTESIAN_POINT('Ctrl Pts',(-4.73222628093364,-72.6487705946061,
-26.9529186924327));
#27521=CARTESIAN_POINT('Ctrl Pts',(-4.59286786251854,-72.9498130615488,
-26.9309675781303));
#27522=CARTESIAN_POINT('Ctrl Pts',(-5.01094311776385,-72.0466856607207,
-26.9968209210375));
#27523=CARTESIAN_POINT('Ctrl Pts',(-5.01017656486953,-72.0463306544706,
-26.9968440313985));
#27524=CARTESIAN_POINT('Ctrl Pts',(-5.00940581101761,-72.0459737040594,
-26.9968671567182));
#27525=CARTESIAN_POINT('Ctrl Pts',(-5.00851041310935,-72.0455590281858,
-26.9968938399568));
#27526=CARTESIAN_POINT('Ctrl Pts',(-5.00757955946722,-72.0451279320846,
-26.9969215797913));
#27527=CARTESIAN_POINT('Ctrl Pts',(-5.00651419661325,-72.0446345417407,
-26.9969531606685));
#27528=CARTESIAN_POINT('Ctrl Pts',(-5.00523178583954,-72.0440406347171,
-26.9969907756178));
#27529=CARTESIAN_POINT('Ctrl Pts',(-5.00388631377784,-72.0434175229001,
-26.9970302402453));
#27530=CARTESIAN_POINT('Ctrl Pts',(-5.00230217741908,-72.0426838837101,
-26.9970763400509));
#27531=CARTESIAN_POINT('Ctrl Pts',(-5.00043760367473,-72.041820379669,-26.9971297520507));
#27532=CARTESIAN_POINT('Ctrl Pts',(-4.99845220009132,-72.0409009180372,
-26.9971866253046));
#27533=CARTESIAN_POINT('Ctrl Pts',(-4.9961491809407,-72.0398343752721,-26.9972517711657));
#27534=CARTESIAN_POINT('Ctrl Pts',(-4.99353288021377,-72.0386227730732,
-26.9973241331438));
#27535=CARTESIAN_POINT('Ctrl Pts',(-4.99066845283999,-72.0372962640566,
-26.9974033578401));
#27536=CARTESIAN_POINT('Ctrl Pts',(-4.98742904190035,-72.0357961260636,
-26.9974911916518));
#27537=CARTESIAN_POINT('Ctrl Pts',(-4.98387738276555,-72.0341514325883,
-26.9975845195401));
#27538=CARTESIAN_POINT('Ctrl Pts',(-4.97950627706432,-72.0321272718358,
-26.9976993802429));
#27539=CARTESIAN_POINT('Ctrl Pts',(-4.97466319276724,-72.0298846097017,
-26.9978224504092));
#27540=CARTESIAN_POINT('Ctrl Pts',(-4.96953845441555,-72.02751161209,-26.9979466068608));
#27541=CARTESIAN_POINT('Ctrl Pts',(-4.96394341208111,-72.0249208413646,
-26.9980821573134));
#27542=CARTESIAN_POINT('Ctrl Pts',(-4.95801831699475,-72.0221773413901,
-26.998218776321));
#27543=CARTESIAN_POINT('Ctrl Pts',(-4.952033932691,-72.0194065054176,-26.998348782628));
#27544=CARTESIAN_POINT('Ctrl Pts',(-4.94749666544916,-72.0173057006142,
-26.998447351391));
#27545=CARTESIAN_POINT('Ctrl Pts',(-4.94292659089731,-72.0151897711979,
-26.998542158666));
#27546=CARTESIAN_POINT('Ctrl Pts',(-4.93841559860224,-72.0131012617228,
-26.9986313749235));
#27547=CARTESIAN_POINT('Ctrl Pts',(-4.93434475476635,-72.0112165331827,
-26.9987118861344));
#27548=CARTESIAN_POINT('Ctrl Pts',(-4.93032259575766,-72.0093543982208,
-26.9987878633368));
#27549=CARTESIAN_POINT('Ctrl Pts',(-4.92638179739851,-72.0075299799368,
-26.9988590242472));
#27550=CARTESIAN_POINT('Ctrl Pts',(-4.92269399034503,-72.0058226856267,
-26.9989256167707));
#27551=CARTESIAN_POINT('Ctrl Pts',(-4.91907780420724,-72.0041485925123,
-26.99898800739));
#27552=CARTESIAN_POINT('Ctrl Pts',(-4.91552145808714,-72.0025022394493,
-26.9990467059966));
#27553=CARTESIAN_POINT('Ctrl Pts',(-4.91192336677503,-72.0008365611231,
-26.9991060936207));
#27554=CARTESIAN_POINT('Ctrl Pts',(-4.90838738253759,-71.9991996731572,
-26.9991617130831));
#27555=CARTESIAN_POINT('Ctrl Pts',(-4.90485074937926,-71.9975625131326,
-26.9992146931177));
#27556=CARTESIAN_POINT('Ctrl Pts',(-4.90140179900313,-71.9959659427703,
-26.9992663596328));
#27557=CARTESIAN_POINT('Ctrl Pts',(-4.89794358042941,-71.994365108323,-26.9993156414398));
#27558=CARTESIAN_POINT('Ctrl Pts',(-4.89442346735378,-71.9927356391644,
-26.9993631288006));
#27559=CARTESIAN_POINT('Ctrl Pts',(-4.89069675220022,-71.9910105333865,
-26.9994134032841));
#27560=CARTESIAN_POINT('Ctrl Pts',(-4.88690099672145,-71.9892534872454,
-26.9994616375389));
#27561=CARTESIAN_POINT('Ctrl Pts',(-4.88302846534461,-71.9874609128104,
-26.9995075736756));
#27562=CARTESIAN_POINT('Ctrl Pts',(-4.87883711126807,-71.9855207570222,
-26.9995572917012));
#27563=CARTESIAN_POINT('Ctrl Pts',(-4.87455631436082,-71.983539211521,-26.9996042784301));
#27564=CARTESIAN_POINT('Ctrl Pts',(-4.87023234098015,-71.9815376862609,
-26.9996476638671));
#27565=CARTESIAN_POINT('Ctrl Pts',(-4.86517549990667,-71.9791969236675,
-26.9996984026762));
#27566=CARTESIAN_POINT('Ctrl Pts',(-4.86006040492235,-71.9768292045297,
-26.9997441449775));
#27567=CARTESIAN_POINT('Ctrl Pts',(-4.85502594174055,-71.9744988084778,
-26.9997837213542));
#27568=CARTESIAN_POINT('Ctrl Pts',(-4.84766089691437,-71.9710896125487,
-26.999841618647));
#27569=CARTESIAN_POINT('Ctrl Pts',(-4.84047595262308,-71.9677637815372,
-26.9998859843948));
#27570=CARTESIAN_POINT('Ctrl Pts',(-4.83398778844191,-71.9647604551997,
-26.9999174873878));
#27571=CARTESIAN_POINT('Ctrl Pts',(-4.82984402883823,-71.9628423375308,
-26.9999376072285));
#27572=CARTESIAN_POINT('Ctrl Pts',(-4.82598611616407,-71.9610565242511,
-26.9999526244651));
#27573=CARTESIAN_POINT('Ctrl Pts',(-4.82251871585362,-71.9594514605147,
-26.9999637790089));
#27574=CARTESIAN_POINT('Ctrl Pts',(-4.81931370885316,-71.9579678589542,
-26.9999740894397));
#27575=CARTESIAN_POINT('Ctrl Pts',(-4.81644333517054,-71.9566391432613,
-26.9999811327487));
#27576=CARTESIAN_POINT('Ctrl Pts',(-4.8139449187002,-71.9554825904982,-26.9999861099321));
#27577=CARTESIAN_POINT('Ctrl Pts',(-4.81176395371457,-71.9544729905736,
-26.9999904547092));
#27578=CARTESIAN_POINT('Ctrl Pts',(-4.80986634322754,-71.9535945432726,
-26.9999932365079));
#27579=CARTESIAN_POINT('Ctrl Pts',(-4.80823665587008,-71.9528401072577,
-26.9999951541055));
#27580=CARTESIAN_POINT('Ctrl Pts',(-4.80667026905868,-71.9521149751527,
-26.9999969972195));
#27581=CARTESIAN_POINT('Ctrl Pts',(-4.80535173946758,-71.95150456664,-26.9999980448942));
#27582=CARTESIAN_POINT('Ctrl Pts',(-4.80422495748871,-71.9509829115286,
-26.9999987249809));
#27583=CARTESIAN_POINT('Ctrl Pts',(-4.80315126323157,-71.9504858339149,
-26.9999993730257));
#27584=CARTESIAN_POINT('Ctrl Pts',(-4.80225182361175,-71.9500694128276,
-26.9999996854072));
#27585=CARTESIAN_POINT('Ctrl Pts',(-4.80143548384865,-71.9496914561439,
-26.9999998528133));
#27586=CARTESIAN_POINT('Ctrl Pts',(-4.80093666763287,-71.9494605095072,
-26.9999999551051));
#27587=CARTESIAN_POINT('Ctrl Pts',(-4.80046803628928,-71.9492435345227,
-27.));
#27588=CARTESIAN_POINT('Ctrl Pts',(-4.8,-71.9490268349807,-27.));
#27589=CARTESIAN_POINT('Ctrl Pts',(-11.7968208397773,-72.0466869089798,
-20.2109458130836));
#27590=CARTESIAN_POINT('Ctrl Pts',(-11.7968651976611,-72.0460055208926,
-20.2094745150254));
#27591=CARTESIAN_POINT('Ctrl Pts',(-11.7969519115959,-72.0445752658204,
-20.2063860590447));
#27592=CARTESIAN_POINT('Ctrl Pts',(-11.7975052989931,-72.0362667659614,
-20.188446468735));
#27593=CARTESIAN_POINT('Ctrl Pts',(-11.7987930505529,-72.011274612559,-20.1344734253031));
#27594=CARTESIAN_POINT('Ctrl Pts',(-11.7996559651957,-71.9844305551918,
-20.0764819862767));
#27595=CARTESIAN_POINT('Ctrl Pts',(-11.8000061190643,-71.9594532702652,
-20.0225220618368));
#27596=CARTESIAN_POINT('Ctrl Pts',(-11.7999927845943,-71.9511381475697,
-20.0045601118682));
#27597=CARTESIAN_POINT('Ctrl Pts',(-11.8,-71.9497084248729,-20.0014721226545));
#27598=CARTESIAN_POINT('Ctrl Pts',(-11.8,-71.9490268349807,-20.));
#27599=CARTESIAN_POINT('Ctrl Pts',(-11.7748696277249,-72.3477293569724,
-20.0715873955272));
#27600=CARTESIAN_POINT('Ctrl Pts',(-11.775019560245,-72.3462468306403,-20.0683107896909));
#27601=CARTESIAN_POINT('Ctrl Pts',(-11.7755113158618,-72.3423634681059,
-20.059760561131));
#27602=CARTESIAN_POINT('Ctrl Pts',(-11.7782701110629,-72.3223183598903,
-20.0159147531201));
#27603=CARTESIAN_POINT('Ctrl Pts',(-11.7845160683301,-72.272988998898,-19.9085744635702));
#27604=CARTESIAN_POINT('Ctrl Pts',(-11.793098520739,-72.2076844580308,-19.7663907236395));
#27605=CARTESIAN_POINT('Ctrl Pts',(-11.7980897330917,-72.1582938607934,
-19.6590311388775));
#27606=CARTESIAN_POINT('Ctrl Pts',(-11.7997839095829,-72.1381225726863,
-19.6151120373436));
#27607=CARTESIAN_POINT('Ctrl Pts',(-11.8,-72.1341926423671,-19.6065422105488));
#27608=CARTESIAN_POINT('Ctrl Pts',(-11.8,-72.1326845566538,-19.6032539761921));
#27609=CARTESIAN_POINT('Ctrl Pts',(-11.7529184156725,-72.6487718049651,
-19.9322289779709));
#27610=CARTESIAN_POINT('Ctrl Pts',(-11.7533738483013,-72.6464941083948,
-19.9271284649557));
#27611=CARTESIAN_POINT('Ctrl Pts',(-11.7544900684487,-72.6425809301834,
-19.9181059391757));
#27612=CARTESIAN_POINT('Ctrl Pts',(-11.7622980156172,-72.615950659827,-19.860231931054));
#27613=CARTESIAN_POINT('Ctrl Pts',(-11.7782324373171,-72.5231684604105,
-19.6622853069392));
#27614=CARTESIAN_POINT('Ctrl Pts',(-11.7937561910005,-72.4384015726793,
-19.4764707261542));
#27615=CARTESIAN_POINT('Ctrl Pts',(-11.7979643479897,-72.3480969257325,
-19.2786158960547));
#27616=CARTESIAN_POINT('Ctrl Pts',(-11.7994070877583,-72.3226741083817,
-19.2206368296666));
#27617=CARTESIAN_POINT('Ctrl Pts',(-11.8,-72.3186768598613,-19.2116122984431));
#27618=CARTESIAN_POINT('Ctrl Pts',(-11.8,-72.3163422783269,-19.2065079523841));
#27619=CARTESIAN_POINT('Ctrl Pts',(-11.73096720362,-72.9498142529578,-19.7928705604145));
#27620=CARTESIAN_POINT('Ctrl Pts',(-11.7319235028288,-72.94677203543,-19.7859815754942));
#27621=CARTESIAN_POINT('Ctrl Pts',(-11.7337970013036,-72.9403554050036,
-19.7715261332556));
#27622=CARTESIAN_POINT('Ctrl Pts',(-11.7456495505882,-72.9035159512033,
-19.687806713427));
#27623=CARTESIAN_POINT('Ctrl Pts',(-11.7734456662866,-72.7907466259382,
-19.4364976352758));
#27624=CARTESIAN_POINT('Ctrl Pts',(-11.7924940627946,-72.6655783935656,
-19.1664460935647));
#27625=CARTESIAN_POINT('Ctrl Pts',(-11.8001369169024,-72.5485937708681,
-18.9151459228174));
#27626=CARTESIAN_POINT('Ctrl Pts',(-11.7998430886325,-72.5097906048016,
-18.8311911573673));
#27627=CARTESIAN_POINT('Ctrl Pts',(-11.8,-72.5031610773555,-18.8166823863373));
#27628=CARTESIAN_POINT('Ctrl Pts',(-11.8,-72.5,-18.8097619285762));
#27629=CARTESIAN_POINT('',(-11.8,-71.9490268349807,-20.));
#27630=CARTESIAN_POINT('',(-11.7968208397773,-72.0466869089798,-20.2109458130836));
#27631=CARTESIAN_POINT('Ctrl Pts',(-11.8,-71.9490268349807,-20.));
#27632=CARTESIAN_POINT('Ctrl Pts',(-11.8,-71.9493819426124,-20.0007669743864));
#27633=CARTESIAN_POINT('Ctrl Pts',(-11.799999888335,-71.9497389941831,-20.0015381483801));
#27634=CARTESIAN_POINT('Ctrl Pts',(-11.7999995768239,-71.9501537654007,
-20.0024340223285));
#27635=CARTESIAN_POINT('Ctrl Pts',(-11.7999992529781,-71.950584960102,-20.003365369739));
#27636=CARTESIAN_POINT('Ctrl Pts',(-11.7999987149954,-71.9510784426209,
-20.0044312864177));
#27637=CARTESIAN_POINT('Ctrl Pts',(-11.7999976675907,-71.9516724317409,
-20.0057143437254));
#27638=CARTESIAN_POINT('Ctrl Pts',(-11.799996568683,-71.9522956285472,-20.0070604916421));
#27639=CARTESIAN_POINT('Ctrl Pts',(-11.7999949097773,-71.9530293412399,
-20.008645404944));
#27640=CARTESIAN_POINT('Ctrl Pts',(-11.7999921086956,-71.9538929058181,
-20.0105108610082));
#27641=CARTESIAN_POINT('Ctrl Pts',(-11.799989126105,-71.9548124290305,-20.0124971978685));
#27642=CARTESIAN_POINT('Ctrl Pts',(-11.7999848409491,-71.9558790177743,
-20.0148012674117));
#27643=CARTESIAN_POINT('Ctrl Pts',(-11.7999783277258,-71.9570906515413,
-20.0174187074598));
#27644=CARTESIAN_POINT('Ctrl Pts',(-11.7999711968429,-71.958417186497,-20.0202843635784));
#27645=CARTESIAN_POINT('Ctrl Pts',(-11.7999613708689,-71.9599173309328,
-20.0235251040395));
#27646=CARTESIAN_POINT('Ctrl Pts',(-11.799947626584,-71.9615620166113,-20.0270781291961));
#27647=CARTESIAN_POINT('Ctrl Pts',(-11.799930711976,-71.963586073436,-20.0314507123044));
#27648=CARTESIAN_POINT('Ctrl Pts',(-11.7999077801487,-71.9658285897296,
-20.0362952824175));
#27649=CARTESIAN_POINT('Ctrl Pts',(-11.7998774465507,-71.9682014257852,
-20.0414214107826));
#27650=CARTESIAN_POINT('Ctrl Pts',(-11.7998443239889,-71.9707924276407,
-20.0470188510583));
#27651=CARTESIAN_POINT('Ctrl Pts',(-11.7998023205844,-71.9735361888576,
-20.052946330571));
#27652=CARTESIAN_POINT('Ctrl Pts',(-11.7997519182459,-71.9763072899415,
-20.0589328686926));
#27653=CARTESIAN_POINT('Ctrl Pts',(-11.7997137069251,-71.9784081335907,
-20.0634714186095));
#27654=CARTESIAN_POINT('Ctrl Pts',(-11.7996707464879,-71.9805241016616,
-20.0680426395345));
#27655=CARTESIAN_POINT('Ctrl Pts',(-11.799623977692,-71.9826126495981,-20.0725546064623));
#27656=CARTESIAN_POINT('Ctrl Pts',(-11.7995817725091,-71.9844974008745,
-20.0766263039694));
#27657=CARTESIAN_POINT('Ctrl Pts',(-11.799536502276,-71.9863595587191,-20.0806491781825));
#27658=CARTESIAN_POINT('Ctrl Pts',(-11.7994888698963,-71.9881839992219,
-20.0845905443789));
#27659=CARTESIAN_POINT('Ctrl Pts',(-11.7994442955327,-71.989891309975,-20.0882788734193));
#27660=CARTESIAN_POINT('Ctrl Pts',(-11.7993976796191,-71.9915654191343,
-20.0918954534738));
#27661=CARTESIAN_POINT('Ctrl Pts',(-11.7993491771455,-71.9932117856955,
-20.0954520633262));
#27662=CARTESIAN_POINT('Ctrl Pts',(-11.7993001195565,-71.9948769950761,
-20.0990493789115));
#27663=CARTESIAN_POINT('Ctrl Pts',(-11.7992491686637,-71.9965134294075,
-20.102584493509));
#27664=CARTESIAN_POINT('Ctrl Pts',(-11.7991955627453,-71.9981501180208,
-20.1061200944543));
#27665=CARTESIAN_POINT('Ctrl Pts',(-11.7991432708341,-71.9997466875428,
-20.1095690294963));
#27666=CARTESIAN_POINT('Ctrl Pts',(-11.7990883172074,-72.0013475043506,
-20.1130270782043));
#27667=CARTESIAN_POINT('Ctrl Pts',(-11.7990297058644,-72.0029769489546,
-20.1165468851023));
#27668=CARTESIAN_POINT('Ctrl Pts',(-11.7989676549683,-72.004702016029,-20.1202732486577));
#27669=CARTESIAN_POINT('Ctrl Pts',(-11.7989014855416,-72.006459015246,-20.1240684980738));
#27670=CARTESIAN_POINT('Ctrl Pts',(-11.798830706444,-72.0082515438015,-20.1279403866504));
#27671=CARTESIAN_POINT('Ctrl Pts',(-11.7987541012368,-72.0101916225281,
-20.1321309858106));
#27672=CARTESIAN_POINT('Ctrl Pts',(-11.7986720719967,-72.0121730910341,
-20.1364108642537));
#27673=CARTESIAN_POINT('Ctrl Pts',(-11.7985851427786,-72.0141745494161,
-20.1407337886868));
#27674=CARTESIAN_POINT('Ctrl Pts',(-11.7984834837389,-72.0165151472244,
-20.1457892160414));
#27675=CARTESIAN_POINT('Ctrl Pts',(-11.7983750765891,-72.0188827135273,
-20.1509027131827));
#27676=CARTESIAN_POINT('Ctrl Pts',(-11.7982629359989,-72.0212129879397,
-20.1559354950726));
#27677=CARTESIAN_POINT('Ctrl Pts',(-11.7980988579961,-72.0246225185231,
-20.1632991873836));
#27678=CARTESIAN_POINT('Ctrl Pts',(-11.7979266789118,-72.0279487283432,
-20.1704825465795));
#27679=CARTESIAN_POINT('Ctrl Pts',(-11.797762638322,-72.0309524055999,-20.176969086863));
#27680=CARTESIAN_POINT('Ctrl Pts',(-11.7976578720253,-72.032870736562,-20.1811117859613));
#27681=CARTESIAN_POINT('Ctrl Pts',(-11.7975566186402,-72.0346567522059,
-20.184968628232));
#27682=CARTESIAN_POINT('Ctrl Pts',(-11.79746327233,-72.0362619878201,-20.1884350084057));
#27683=CARTESIAN_POINT('Ctrl Pts',(-11.7973769893237,-72.0377457588903,
-20.1916390954408));
#27684=CARTESIAN_POINT('Ctrl Pts',(-11.7972975249092,-72.0390746155401,
-20.1945085882328));
#27685=CARTESIAN_POINT('Ctrl Pts',(-11.7972272049842,-72.0402312692395,
-20.1970061974383));
#27686=CARTESIAN_POINT('Ctrl Pts',(-11.7971658232559,-72.0412409034669,
-20.1991863415397));
#27687=CARTESIAN_POINT('Ctrl Pts',(-11.7971114179676,-72.0421193686887,
-20.2010832179952));
#27688=CARTESIAN_POINT('Ctrl Pts',(-11.7970642228539,-72.0428738025906,
-20.2027122622304));
#27689=CARTESIAN_POINT('Ctrl Pts',(-11.7970188610415,-72.0435989303922,
-20.2042780259932));
#27690=CARTESIAN_POINT('Ctrl Pts',(-11.7969801733989,-72.0442093167846,
-20.2055960182921));
#27691=CARTESIAN_POINT('Ctrl Pts',(-11.7969468970578,-72.0447309306672,
-20.206722325243));
#27692=CARTESIAN_POINT('Ctrl Pts',(-11.7969151886715,-72.045227966516,-20.2077955615005));
#27693=CARTESIAN_POINT('Ctrl Pts',(-11.7968883962598,-72.0456443292891,
-20.208694601408));
#27694=CARTESIAN_POINT('Ctrl Pts',(-11.7968639638509,-72.0460222115476,
-20.2095105519188));
#27695=CARTESIAN_POINT('Ctrl Pts',(-11.7968490293866,-72.0462531944641,
-20.2100093068207));
#27696=CARTESIAN_POINT('Ctrl Pts',(-11.7968349480525,-72.0464701896551,
-20.210477858437));
#27697=CARTESIAN_POINT('Ctrl Pts',(-11.7968208397773,-72.0466869089798,
-20.2109458130836));
#27698=CARTESIAN_POINT('',(-11.73096720362,-72.9498142529578,-19.7928705604145));
#27699=CARTESIAN_POINT('Ctrl Pts',(-11.73096720362,-72.9498142529578,-19.7928705604145));
#27700=CARTESIAN_POINT('Ctrl Pts',(-11.7529184156725,-72.6487718049651,
-19.9322289779709));
#27701=CARTESIAN_POINT('Ctrl Pts',(-11.7748696277249,-72.3477293569724,
-20.0715873955272));
#27702=CARTESIAN_POINT('Ctrl Pts',(-11.7968208397773,-72.0466869089798,
-20.2109458130836));
#27703=CARTESIAN_POINT('',(-11.8,-72.5,-18.8097619285762));
#27704=CARTESIAN_POINT('Ctrl Pts',(-11.73096720362,-72.9498142529578,-19.7928705604145));
#27705=CARTESIAN_POINT('Ctrl Pts',(-11.7313015196475,-72.948750713357,-19.7904622157761));
#27706=CARTESIAN_POINT('Ctrl Pts',(-11.7316352664094,-72.9476850547636,
-19.7880498402146));
#27707=CARTESIAN_POINT('Ctrl Pts',(-11.7319930278409,-72.9465377567631,
-19.7854527057828));
#27708=CARTESIAN_POINT('Ctrl Pts',(-11.7323595526967,-72.9453623555119,
-19.7827919541218));
#27709=CARTESIAN_POINT('Ctrl Pts',(-11.7327512682097,-72.9441013208732,
-19.7799374057456));
#27710=CARTESIAN_POINT('Ctrl Pts',(-11.7331869939848,-72.9426906823876,
-19.7767444366006));
#27711=CARTESIAN_POINT('Ctrl Pts',(-11.7336348584884,-72.9412407454291,
-19.7734625156706));
#27712=CARTESIAN_POINT('Ctrl Pts',(-11.7341292070935,-72.9396328168219,
-19.7698231983777));
#27713=CARTESIAN_POINT('Ctrl Pts',(-11.7346827218845,-72.9378190122941,
-19.7657193035655));
#27714=CARTESIAN_POINT('Ctrl Pts',(-11.7352541156892,-72.9359466202874,
-19.7614828493476));
#27715=CARTESIAN_POINT('Ctrl Pts',(-11.7358885391894,-72.9338549102333,
-19.7567514881668));
#27716=CARTESIAN_POINT('Ctrl Pts',(-11.7365920277446,-72.9315128570745,
-19.7514573835512));
#27717=CARTESIAN_POINT('Ctrl Pts',(-11.737339030065,-72.9290259379468,-19.7458358160034));
#27718=CARTESIAN_POINT('Ctrl Pts',(-11.7381638939142,-72.9262567549538,
-19.7395797634214));
#27719=CARTESIAN_POINT('Ctrl Pts',(-11.7390652426951,-72.9231917145537,
-19.7326623884211));
#27720=CARTESIAN_POINT('Ctrl Pts',(-11.7400142162781,-72.9199647258095,
-19.7253795182624));
#27721=CARTESIAN_POINT('Ctrl Pts',(-11.7410478975251,-72.9164098863763,
-19.7173638520341));
#27722=CARTESIAN_POINT('Ctrl Pts',(-11.742156091357,-72.9125358265191,-19.7086402756966));
#27723=CARTESIAN_POINT('Ctrl Pts',(-11.743343246297,-72.9083857318654,-19.6992951264596));
#27724=CARTESIAN_POINT('Ctrl Pts',(-11.7446157812005,-72.9038694321553,
-19.6891379476566));
#27725=CARTESIAN_POINT('Ctrl Pts',(-11.7459531151839,-72.8990232934177,
-19.678257641115));
#27726=CARTESIAN_POINT('Ctrl Pts',(-11.7474361285517,-72.8936492517657,
-19.6661921135459));
#27727=CARTESIAN_POINT('Ctrl Pts',(-11.7489985853597,-72.8878697945666,
-19.6532379065394));
#27728=CARTESIAN_POINT('Ctrl Pts',(-11.7506057804669,-72.881762844808,-19.6395787832203));
#27729=CARTESIAN_POINT('Ctrl Pts',(-11.7525799686944,-72.8742614106234,
-19.6228006830806));
#27730=CARTESIAN_POINT('Ctrl Pts',(-11.7546209594929,-72.8662663671094,
-19.604960507791));
#27731=CARTESIAN_POINT('Ctrl Pts',(-11.7566625088008,-72.8579585666724,
-19.586474830845));
#27732=CARTESIAN_POINT('Ctrl Pts',(-11.7587486675852,-72.8494692341864,
-19.5675852271509));
#27733=CARTESIAN_POINT('Ctrl Pts',(-11.7608345555821,-72.8406557779562,
-19.5480271717187));
#27734=CARTESIAN_POINT('Ctrl Pts',(-11.7628608882688,-72.8317197937618,
-19.5282555924746));
#27735=CARTESIAN_POINT('Ctrl Pts',(-11.7644778516186,-72.8245890994631,
-19.5124783614135));
#27736=CARTESIAN_POINT('Ctrl Pts',(-11.7660570732259,-72.8173810768957,
-19.4965664860538));
#27737=CARTESIAN_POINT('Ctrl Pts',(-11.7675779301993,-72.8101854587048,
-19.4807189446334));
#27738=CARTESIAN_POINT('Ctrl Pts',(-11.7689362640305,-72.8037587849308,
-19.4665649169842));
#27739=CARTESIAN_POINT('Ctrl Pts',(-11.7702481416314,-72.797342265795,-19.4524626966761));
#27740=CARTESIAN_POINT('Ctrl Pts',(-11.7715056463165,-72.7909830456549,
-19.4385150048574));
#27741=CARTESIAN_POINT('Ctrl Pts',(-11.7726775448823,-72.7850567369498,
-19.4255168186616));
#27742=CARTESIAN_POINT('Ctrl Pts',(-11.7738022936455,-72.7791803623659,
-19.4126531659137));
#27743=CARTESIAN_POINT('Ctrl Pts',(-11.7748785745449,-72.7733737191987,
-19.3999657098098));
#27744=CARTESIAN_POINT('Ctrl Pts',(-11.7759007008184,-72.7678592456579,
-19.3879166413602));
#27745=CARTESIAN_POINT('Ctrl Pts',(-11.7768791728643,-72.7624077892709,
-19.3760267312504));
#27746=CARTESIAN_POINT('Ctrl Pts',(-11.7778167135231,-72.7570170446327,
-19.3642888201112));
#27747=CARTESIAN_POINT('Ctrl Pts',(-11.7787167543063,-72.7518419197138,
-19.3530204034994));
#27748=CARTESIAN_POINT('Ctrl Pts',(-11.7795791232979,-72.7467228466605,
-19.3418922673075));
#27749=CARTESIAN_POINT('Ctrl Pts',(-11.7804091012626,-72.7416379376232,
-19.3308543416171));
#27750=CARTESIAN_POINT('Ctrl Pts',(-11.7812615549807,-72.7364153295549,
-19.3195175095628));
#27751=CARTESIAN_POINT('Ctrl Pts',(-11.7820798790364,-72.7312290756134,
-19.3082765101024));
#27752=CARTESIAN_POINT('Ctrl Pts',(-11.78287228708,-72.7260304851342,-19.2970224013524));
#27753=CARTESIAN_POINT('Ctrl Pts',(-11.7836281622423,-72.7210715685085,
-19.2862871477848));
#27754=CARTESIAN_POINT('Ctrl Pts',(-11.7843609633582,-72.7160978816426,
-19.2755321855914));
#27755=CARTESIAN_POINT('Ctrl Pts',(-11.7850752081796,-72.7110725611027,
-19.2646751402817));
#27756=CARTESIAN_POINT('Ctrl Pts',(-11.7858149458742,-72.7058678764904,
-19.2534305845943));
#27757=CARTESIAN_POINT('Ctrl Pts',(-11.7865346992853,-72.7006078834654,
-19.2420767205995));
#27758=CARTESIAN_POINT('Ctrl Pts',(-11.787234971241,-72.6952745255222,-19.2305723846674));
#27759=CARTESIAN_POINT('Ctrl Pts',(-11.787983905607,-72.6895705486344,-19.2182686040163));
#27760=CARTESIAN_POINT('Ctrl Pts',(-11.7887104701913,-72.6837826658412,
-19.2057927574211));
#27761=CARTESIAN_POINT('Ctrl Pts',(-11.7894114938235,-72.6779140299877,
-19.1931496137544));
#27762=CARTESIAN_POINT('Ctrl Pts',(-11.7901552177242,-72.67168792783,-19.1797363596303));
#27763=CARTESIAN_POINT('Ctrl Pts',(-11.790870062336,-72.6653710751155,-19.1661351349512));
#27764=CARTESIAN_POINT('Ctrl Pts',(-11.7915498844441,-72.6589935288453,
-19.1524086643696));
#27765=CARTESIAN_POINT('Ctrl Pts',(-11.7922885192423,-72.6520642490451,
-19.1374946909855));
#27766=CARTESIAN_POINT('Ctrl Pts',(-11.7929856244291,-72.6450635375576,
-19.1224333550758));
#27767=CARTESIAN_POINT('Ctrl Pts',(-11.7936332018617,-72.6380574456386,
-19.1073643771971));
#27768=CARTESIAN_POINT('Ctrl Pts',(-11.7943843329216,-72.6299310147553,
-19.0898857302383));
#27769=CARTESIAN_POINT('Ctrl Pts',(-11.7950684833757,-72.6217977656785,
-19.0723977162336));
#27770=CARTESIAN_POINT('Ctrl Pts',(-11.7956775773033,-72.6137918483554,
-19.0551850309453));
#27771=CARTESIAN_POINT('Ctrl Pts',(-11.7964581312637,-72.6035322640937,
-19.0331269721424));
#27772=CARTESIAN_POINT('Ctrl Pts',(-11.7971144717794,-72.5934842779128,
-19.0115263327855));
#27773=CARTESIAN_POINT('Ctrl Pts',(-11.7976485571115,-72.5839571282364,
-18.991040307301));
#27774=CARTESIAN_POINT('Ctrl Pts',(-11.7980302737727,-72.5771479695768,
-18.9763987195685));
#27775=CARTESIAN_POINT('Ctrl Pts',(-11.798350091132,-72.5706057723494,-18.9623284432994));
#27776=CARTESIAN_POINT('Ctrl Pts',(-11.7986154805682,-72.5644332321203,
-18.9490480921655));
#27777=CARTESIAN_POINT('Ctrl Pts',(-11.7988537013714,-72.5588925914945,
-18.9371272864217));
#27778=CARTESIAN_POINT('Ctrl Pts',(-11.7990482195448,-72.5536501203106,
-18.9258436471241));
#27779=CARTESIAN_POINT('Ctrl Pts',(-11.7992071495588,-72.548763948896,-18.9153211964204));
#27780=CARTESIAN_POINT('Ctrl Pts',(-11.7993555434031,-72.5442017032746,
-18.9054963252532));
#27781=CARTESIAN_POINT('Ctrl Pts',(-11.7994730024161,-72.5399502820446,
-18.8963354982137));
#27782=CARTESIAN_POINT('Ctrl Pts',(-11.7995670103527,-72.5360386107081,
-18.8879006581774));
#27783=CARTESIAN_POINT('Ctrl Pts',(-11.799656382681,-72.5323198270885,-18.8798817470105));
#27784=CARTESIAN_POINT('Ctrl Pts',(-11.7997246147799,-72.528908256622,-18.8725193061859));
#27785=CARTESIAN_POINT('Ctrl Pts',(-11.7997779466319,-72.5258091223535,
-18.8658247654831));
#27786=CARTESIAN_POINT('Ctrl Pts',(-11.7998291813466,-72.5228318535359,
-18.8593934703034));
#27787=CARTESIAN_POINT('Ctrl Pts',(-11.7998666928443,-72.5201430448025,
-18.853578828993));
#27788=CARTESIAN_POINT('Ctrl Pts',(-11.7998952486479,-72.5177269028185,
-18.8483473576186));
#27789=CARTESIAN_POINT('Ctrl Pts',(-11.7999224505255,-72.5154253181936,
-18.8433639277702));
#27790=CARTESIAN_POINT('Ctrl Pts',(-11.7999415314462,-72.5133711920832,
-18.8389097591737));
#27791=CARTESIAN_POINT('Ctrl Pts',(-11.7999556780829,-72.5115309924458,
-18.8349133524625));
#27792=CARTESIAN_POINT('Ctrl Pts',(-11.7999695052011,-72.5097323559027,
-18.8310072093431));
#27793=CARTESIAN_POINT('Ctrl Pts',(-11.7999786158405,-72.5081381840189,
-18.8275385858994));
#27794=CARTESIAN_POINT('Ctrl Pts',(-11.7999850514837,-72.5066966652379,
-18.8243967636039));
#27795=CARTESIAN_POINT('Ctrl Pts',(-11.7999912849267,-72.5053004372806,
-18.8213536536676));
#27796=CARTESIAN_POINT('Ctrl Pts',(-11.7999950012486,-72.5040474593205,
-18.8186172172743));
#27797=CARTESIAN_POINT('Ctrl Pts',(-11.7999972537808,-72.5028703048568,
-18.8160431764752));
#27798=CARTESIAN_POINT('Ctrl Pts',(-11.7999991536502,-72.5018774490286,
-18.8138721347909));
#27799=CARTESIAN_POINT('Ctrl Pts',(-11.8,-72.500938234387,-18.8118159787353));
#27800=CARTESIAN_POINT('Ctrl Pts',(-11.8,-72.5,-18.8097619285762));
#27801=CARTESIAN_POINT('',(-11.8,-72.2245134174903,-19.4048809642881));
#27802=CARTESIAN_POINT('Ctrl Pts',(-11.73096720362,-72.9498142529578,-19.7928705604145));
#27803=CARTESIAN_POINT('Ctrl Pts',(-11.6459067968618,-73.2204118420674,
-20.405628423336));
#27804=CARTESIAN_POINT('Ctrl Pts',(-11.3040150424387,-73.7466604863582,
-21.7070034589623));
#27805=CARTESIAN_POINT('Ctrl Pts',(-10.6578917243185,-74.000000000005,-22.9273203194824));
#27806=CARTESIAN_POINT('Ctrl Pts',(-10.299999999979,-74.,-23.4706975310694));
#27807=CARTESIAN_POINT('Ctrl Pts',(-11.7529184156725,-72.6487718049651,
-19.9322289779709));
#27808=CARTESIAN_POINT('Ctrl Pts',(-11.6900562551077,-72.9237214947494,
-20.5448956110034));
#27809=CARTESIAN_POINT('Ctrl Pts',(-11.3929734933996,-73.4750028661316,
-21.8418300905598));
#27810=CARTESIAN_POINT('Ctrl Pts',(-10.7749647057687,-73.7841592833289,
-23.0483683735484));
#27811=CARTESIAN_POINT('Ctrl Pts',(-10.4245617157746,-73.8157835059031,
-23.5830861153787));
#27812=CARTESIAN_POINT('Ctrl Pts',(-11.7748696277249,-72.3477293569724,
-20.0715873955272));
#27813=CARTESIAN_POINT('Ctrl Pts',(-11.7342057133535,-72.6270311474313,
-20.6841627986708));
#27814=CARTESIAN_POINT('Ctrl Pts',(-11.4819319443604,-73.203345245905,-21.9766567221572));
#27815=CARTESIAN_POINT('Ctrl Pts',(-10.8920376872188,-73.5683185666529,
-23.1694164276145));
#27816=CARTESIAN_POINT('Ctrl Pts',(-10.5491234315702,-73.6315670118062,
-23.6954746996879));
#27817=CARTESIAN_POINT('Ctrl Pts',(-11.7968208397773,-72.0466869089798,
-20.2109458130836));
#27818=CARTESIAN_POINT('Ctrl Pts',(-11.7783551715994,-72.3303408001132,
-20.8234299863382));
#27819=CARTESIAN_POINT('Ctrl Pts',(-11.5708903953213,-72.9316876256785,
-22.1114833537547));
#27820=CARTESIAN_POINT('Ctrl Pts',(-11.009110668669,-73.3524778499768,-23.2904644816805));
#27821=CARTESIAN_POINT('Ctrl Pts',(-10.6736851473658,-73.4473505177094,
-23.8078632839972));
#27822=CARTESIAN_POINT('',(-10.6736851473658,-73.4473505177094,-23.8078632839972));
#27823=CARTESIAN_POINT('Ctrl Pts',(-11.7968208397773,-72.0466869089798,
-20.2109458130836));
#27824=CARTESIAN_POINT('Ctrl Pts',(-11.7783551715994,-72.3303408001132,
-20.8234299863382));
#27825=CARTESIAN_POINT('Ctrl Pts',(-11.5708903953213,-72.9316876256785,
-22.1114833537547));
#27826=CARTESIAN_POINT('Ctrl Pts',(-11.009110668669,-73.3524778499768,-23.2904644816805));
#27827=CARTESIAN_POINT('Ctrl Pts',(-10.6736851473658,-73.4473505177094,
-23.8078632839972));
#27828=CARTESIAN_POINT('',(-10.2999999999876,-74.,-23.4706975310751));
#27829=CARTESIAN_POINT('',(-10.6736851473658,-73.4473505177094,-23.8078632839972));
#27830=CARTESIAN_POINT('Ctrl Pts',(-10.299999999979,-74.,-23.4706975310694));
#27831=CARTESIAN_POINT('Ctrl Pts',(-10.6578917243185,-74.000000000005,-22.9273203194824));
#27832=CARTESIAN_POINT('Ctrl Pts',(-11.3040150424387,-73.7466604863582,
-21.7070034589623));
#27833=CARTESIAN_POINT('Ctrl Pts',(-11.6459067968618,-73.2204118420674,
-20.405628423336));
#27834=CARTESIAN_POINT('Ctrl Pts',(-11.73096720362,-72.9498142529578,-19.7928705604145));
#27835=CARTESIAN_POINT('Origin',(-4.79999999999999,-73.75,-20.));
#27836=CARTESIAN_POINT('',(-9.13012701892219,-73.5,-25.5));
#27837=CARTESIAN_POINT('',(-8.82083223185632,-74.,-25.1071428571429));
#27838=CARTESIAN_POINT('',(-9.13012701892219,-73.5,-25.5));
#27839=CARTESIAN_POINT('',(-9.90714285714286,-74.,-24.0208322318563));
#27840=CARTESIAN_POINT('Origin',(-4.79999999999999,-74.,-20.));
#27841=CARTESIAN_POINT('',(-10.3,-73.5,-24.3301270189222));
#27842=CARTESIAN_POINT('',(-9.90714285714286,-74.,-24.0208322318563));
#27843=CARTESIAN_POINT('Origin',(-4.79999999999999,-73.5,-20.));
#27844=CARTESIAN_POINT('Ctrl Pts',(-10.299999999979,-74.,-23.4706975310694));
#27845=CARTESIAN_POINT('Ctrl Pts',(-10.1730966676381,-74.,-23.6633713879345));
#27846=CARTESIAN_POINT('Ctrl Pts',(-10.0446625272125,-74.,-23.8461587910824));
#27847=CARTESIAN_POINT('Ctrl Pts',(-9.90714285714286,-74.,-24.0208322318563));
#27848=CARTESIAN_POINT('Ctrl Pts',(-10.4245617157746,-73.8157835059031,
-23.5830861153787));
#27849=CARTESIAN_POINT('Ctrl Pts',(-10.3003137824799,-73.8269970069562,
-23.7726894470159));
#27850=CARTESIAN_POINT('Ctrl Pts',(-10.1728443653613,-73.8333333333333,
-23.9527761154313));
#27851=CARTESIAN_POINT('Ctrl Pts',(-10.0380952380952,-73.8333333333333,
-24.1239304942116));
#27852=CARTESIAN_POINT('Ctrl Pts',(-10.5491234315702,-73.6315670118063,
-23.6954746996879));
#27853=CARTESIAN_POINT('Ctrl Pts',(-10.4275308973216,-73.6539940139125,
-23.8820075060973));
#27854=CARTESIAN_POINT('Ctrl Pts',(-10.3010262035101,-73.6666666666667,
-24.0593934397802));
#27855=CARTESIAN_POINT('Ctrl Pts',(-10.1690476190476,-73.6666666666667,
-24.2270287565669));
#27856=CARTESIAN_POINT('Ctrl Pts',(-10.6736851473658,-73.4473505177094,
-23.8078632839972));
#27857=CARTESIAN_POINT('Ctrl Pts',(-10.5547480121633,-73.4809910208687,
-23.9913255651787));
#27858=CARTESIAN_POINT('Ctrl Pts',(-10.4292080416588,-73.5,-24.1660107641291));
#27859=CARTESIAN_POINT('Ctrl Pts',(-10.3,-73.5,-24.3301270189222));
#27860=CARTESIAN_POINT('Ctrl Pts',(-9.90714285714286,-74.,-24.0208322318563));
#27861=CARTESIAN_POINT('Ctrl Pts',(-10.0446625272125,-74.,-23.8461587910824));
#27862=CARTESIAN_POINT('Ctrl Pts',(-10.1730966676381,-74.,-23.6633713879345));
#27863=CARTESIAN_POINT('Ctrl Pts',(-10.299999999979,-74.,-23.4706975310694));
#27864=CARTESIAN_POINT('Ctrl Pts',(-10.6736851473658,-73.4473505177094,
-23.8078632839972));
#27865=CARTESIAN_POINT('Ctrl Pts',(-10.5547480121633,-73.4809910208687,
-23.9913255651787));
#27866=CARTESIAN_POINT('Ctrl Pts',(-10.4292080416588,-73.5,-24.1660107641291));
#27867=CARTESIAN_POINT('Ctrl Pts',(-10.3,-73.5,-24.3301270189222));
#27868=CARTESIAN_POINT('Ctrl Pts',(-8.27069753274498,-74.,-25.4999999988754));
#27869=CARTESIAN_POINT('Ctrl Pts',(-7.86775357562108,-74.000000000199,-25.7653963103419));
#27870=CARTESIAN_POINT('Ctrl Pts',(-7.41892233716379,-73.9255855959792,
-26.0143834333207));
#27871=CARTESIAN_POINT('Ctrl Pts',(-6.64131213535275,-73.7333039309982,
-26.3751847566866));
#27872=CARTESIAN_POINT('Ctrl Pts',(-6.23069752441905,-73.6032053694849,
-26.5355631282739));
#27873=CARTESIAN_POINT('Ctrl Pts',(-5.3994360061265,-73.2960267407261,-26.7866346555581));
#27874=CARTESIAN_POINT('Ctrl Pts',(-4.97871567190643,-73.1202058398724,
-26.8774059891363));
#27875=CARTESIAN_POINT('Ctrl Pts',(-4.59286786251854,-72.9498130615488,
-26.9309675781303));
#27876=CARTESIAN_POINT('Ctrl Pts',(-8.38308611702755,-73.8157835060006,
-25.6245617146941));
#27877=CARTESIAN_POINT('Ctrl Pts',(-7.98659795770256,-73.792224809411,-25.8845123595968));
#27878=CARTESIAN_POINT('Ctrl Pts',(-7.54321375147387,-73.6962979999651,
-26.1239924943787));
#27879=CARTESIAN_POINT('Ctrl Pts',(-6.77293317326111,-73.4735100646501,
-26.4648563557158));
#27880=CARTESIAN_POINT('Ctrl Pts',(-6.36525357393195,-73.3302738061139,
-26.6131752565609));
#27881=CARTESIAN_POINT('Ctrl Pts',(-5.53781831770394,-73.0038693973692,
-26.8373085713286));
#27882=CARTESIAN_POINT('Ctrl Pts',(-5.11803369719418,-72.8218328925055,
-26.9133546198602));
#27883=CARTESIAN_POINT('Ctrl Pts',(-4.73222628093364,-72.6487705946061,
-26.9529186924327));
#27884=CARTESIAN_POINT('Ctrl Pts',(-8.49547470131012,-73.6315670120013,
-25.7491234305128));
#27885=CARTESIAN_POINT('Ctrl Pts',(-8.10533935942276,-73.5847724307058,
-26.0033054887914));
#27886=CARTESIAN_POINT('Ctrl Pts',(-7.66749386372855,-73.4670506442876,
-26.2335668887596));
#27887=CARTESIAN_POINT('Ctrl Pts',(-6.90453529773527,-73.2137792063844,
-26.5544816958254));
#27888=CARTESIAN_POINT('Ctrl Pts',(-6.49978151201769,-73.0574412945255,
-26.6907208978012));
#27889=CARTESIAN_POINT('Ctrl Pts',(-5.6762040020745,-72.7117043334441,-26.8879935435987));
#27890=CARTESIAN_POINT('Ctrl Pts',(-5.25729945114597,-72.523672254769,-26.9492448165541));
#27891=CARTESIAN_POINT('Ctrl Pts',(-4.87158469934875,-72.3477281276634,
-26.9748698067351));
#27892=CARTESIAN_POINT('Ctrl Pts',(-8.60786328559269,-73.4473505180019,
-25.8736851463315));
#27893=CARTESIAN_POINT('Ctrl Pts',(-8.22418374150425,-73.3769972399179,
-26.1224215380463));
#27894=CARTESIAN_POINT('Ctrl Pts',(-7.79178527803863,-73.2377630482735,
-26.3431759498177));
#27895=CARTESIAN_POINT('Ctrl Pts',(-7.03615633564364,-72.9539853400363,
-26.6441532948547));
#27896=CARTESIAN_POINT('Ctrl Pts',(-6.63433756153059,-72.7845097311546,
-26.7683330260882));
#27897=CARTESIAN_POINT('Ctrl Pts',(-5.81458631365194,-72.4195469900871,
-26.9386674593692));
#27898=CARTESIAN_POINT('Ctrl Pts',(-5.39661747643372,-72.2252993074021,
-26.985193447278));
#27899=CARTESIAN_POINT('Ctrl Pts',(-5.01094311776385,-72.0466856607207,
-26.9968209210375));
#27900=CARTESIAN_POINT('',(-8.27069753304877,-74.,-25.4999999993376));
#27901=CARTESIAN_POINT('Ctrl Pts',(-4.59286786251854,-72.9498130615488,
-26.9309675781303));
#27902=CARTESIAN_POINT('Ctrl Pts',(-4.97871567190643,-73.1202058398724,
-26.8774059891363));
#27903=CARTESIAN_POINT('Ctrl Pts',(-5.3994360061265,-73.2960267407261,-26.7866346555581));
#27904=CARTESIAN_POINT('Ctrl Pts',(-6.23069752441905,-73.6032053694849,
-26.5355631282739));
#27905=CARTESIAN_POINT('Ctrl Pts',(-6.64131213535275,-73.7333039309982,
-26.3751847566866));
#27906=CARTESIAN_POINT('Ctrl Pts',(-7.41892233716379,-73.9255855959792,
-26.0143834333207));
#27907=CARTESIAN_POINT('Ctrl Pts',(-7.86775357562108,-74.000000000199,-25.7653963103419));
#27908=CARTESIAN_POINT('Ctrl Pts',(-8.27069753274498,-74.,-25.4999999988754));
#27909=CARTESIAN_POINT('',(-8.60786328559223,-73.4473505180018,-25.8736851463318));
#27910=CARTESIAN_POINT('',(-8.27069753304877,-74.,-25.4999999993376));
#27911=CARTESIAN_POINT('Ctrl Pts',(-8.60786328559269,-73.4473505180019,
-25.8736851463315));
#27912=CARTESIAN_POINT('Ctrl Pts',(-8.22418374150425,-73.3769972399179,
-26.1224215380463));
#27913=CARTESIAN_POINT('Ctrl Pts',(-7.79178527803863,-73.2377630482735,
-26.3431759498177));
#27914=CARTESIAN_POINT('Ctrl Pts',(-7.03615633564364,-72.9539853400363,
-26.6441532948547));
#27915=CARTESIAN_POINT('Ctrl Pts',(-6.63433756153059,-72.7845097311546,
-26.7683330260882));
#27916=CARTESIAN_POINT('Ctrl Pts',(-5.81458631365194,-72.4195469900871,
-26.9386674593692));
#27917=CARTESIAN_POINT('Ctrl Pts',(-5.39661747643372,-72.2252993074021,
-26.985193447278));
#27918=CARTESIAN_POINT('Ctrl Pts',(-5.01094311776385,-72.0466856607207,
-26.9968209210375));
#27919=CARTESIAN_POINT('Ctrl Pts',(-8.82083223185632,-74.,-25.1071428571429));
#27920=CARTESIAN_POINT('Ctrl Pts',(-8.6524411521674,-74.,-25.2397164505804));
#27921=CARTESIAN_POINT('Ctrl Pts',(-8.46780983228827,-74.,-25.3701733162485));
#27922=CARTESIAN_POINT('Ctrl Pts',(-8.2706975327445,-74.,-25.4999999988757));
#27923=CARTESIAN_POINT('Ctrl Pts',(-8.92393049421161,-73.8333333333333,
-25.2380952380952));
#27924=CARTESIAN_POINT('Ctrl Pts',(-8.75893190880213,-73.8333333333333,
-25.3679979349617));
#27925=CARTESIAN_POINT('Ctrl Pts',(-8.57705715860084,-73.8272553216869,
-25.4974516009823));
#27926=CARTESIAN_POINT('Ctrl Pts',(-8.38308611702708,-73.8157835060006,
-25.6245617146944));
#27927=CARTESIAN_POINT('Ctrl Pts',(-9.0270287565669,-73.6666666666667,-25.3690476190476));
#27928=CARTESIAN_POINT('Ctrl Pts',(-8.86542266543687,-73.6666666666667,
-25.496279419343));
#27929=CARTESIAN_POINT('Ctrl Pts',(-8.68630448491342,-73.6545106433737,
-25.6247298857161));
#27930=CARTESIAN_POINT('Ctrl Pts',(-8.49547470130966,-73.6315670120012,
-25.7491234305131));
#27931=CARTESIAN_POINT('Ctrl Pts',(-9.13012701892219,-73.5,-25.5));
#27932=CARTESIAN_POINT('Ctrl Pts',(-8.97191342207161,-73.5,-25.6245609037243));
#27933=CARTESIAN_POINT('Ctrl Pts',(-8.79555181122599,-73.4817659650606,
-25.7520081704499));
#27934=CARTESIAN_POINT('Ctrl Pts',(-8.60786328559223,-73.4473505180018,
-25.8736851463318));
#27935=CARTESIAN_POINT('Ctrl Pts',(-8.2706975327445,-74.,-25.4999999988757));
#27936=CARTESIAN_POINT('Ctrl Pts',(-8.46780983228827,-74.,-25.3701733162485));
#27937=CARTESIAN_POINT('Ctrl Pts',(-8.6524411521674,-74.,-25.2397164505804));
#27938=CARTESIAN_POINT('Ctrl Pts',(-8.82083223185632,-74.,-25.1071428571429));
#27939=CARTESIAN_POINT('Ctrl Pts',(-9.13012701892219,-73.5,-25.5));
#27940=CARTESIAN_POINT('Ctrl Pts',(-8.97191342207161,-73.5,-25.6245609037243));
#27941=CARTESIAN_POINT('Ctrl Pts',(-8.79555181122599,-73.4817659650606,
-25.7520081704499));
#27942=CARTESIAN_POINT('Ctrl Pts',(-8.60786328559223,-73.4473505180018,
-25.8736851463318));
#27943=CARTESIAN_POINT('Origin',(5.2,-72.5,-25.5));
#27944=CARTESIAN_POINT('',(34.9928690003034,-72.9498135639887,-26.9309674201923));
#27945=CARTESIAN_POINT('Ctrl Pts',(34.9928690003034,-72.9498135639887,-26.9309674201923));
#27946=CARTESIAN_POINT('Ctrl Pts',(34.9904606339408,-72.948750014595,-26.9313017387355));
#27947=CARTESIAN_POINT('Ctrl Pts',(34.98804823666,-72.9476843461928,-26.9316354879942));
#27948=CARTESIAN_POINT('Ctrl Pts',(34.9854510809667,-72.9465370382985,-26.9319932518792));
#27949=CARTESIAN_POINT('Ctrl Pts',(34.9827903074055,-72.9453616268591,-26.9323597792649));
#27950=CARTESIAN_POINT('Ctrl Pts',(34.9799357375926,-72.944100581936,-26.9327514972644));
#27951=CARTESIAN_POINT('Ctrl Pts',(34.9767427478805,-72.9426899331038,-26.9331872254275));
#27952=CARTESIAN_POINT('Ctrl Pts',(34.9734608056225,-72.9412399854274,-26.9336350924113));
#27953=CARTESIAN_POINT('Ctrl Pts',(34.9698214678795,-72.9396320460192,-26.9341294433976));
#27954=CARTESIAN_POINT('Ctrl Pts',(34.9657175538563,-72.9378182307483,-26.9346829603869));
#27955=CARTESIAN_POINT('Ctrl Pts',(34.9614810794814,-72.9359458275077,-26.9352543565048));
#27956=CARTESIAN_POINT('Ctrl Pts',(34.9567496993881,-72.9338541062487,-26.9358887821325));
#27957=CARTESIAN_POINT('Ctrl Pts',(34.9514555774257,-72.9315120421697,-26.9365922725194));
#27958=CARTESIAN_POINT('Ctrl Pts',(34.9458339906315,-72.9290251110807,-26.9373392768946));
#27959=CARTESIAN_POINT('Ctrl Pts',(34.9395779203818,-72.9262559163651,-26.9381641424873));
#27960=CARTESIAN_POINT('Ctrl Pts',(34.9326605296007,-72.9231908648904,-26.9390654925587));
#27961=CARTESIAN_POINT('Ctrl Pts',(34.9253776414208,-72.9199638638632,-26.9400144676838));
#27962=CARTESIAN_POINT('Ctrl Pts',(34.9173619589799,-72.9164090127403,-26.9410481500021));
#27963=CARTESIAN_POINT('Ctrl Pts',(34.9086383685528,-72.9125349423719,-26.9421563442714));
#27964=CARTESIAN_POINT('Ctrl Pts',(34.8992932010295,-72.9083848350403,-26.9433435000854));
#27965=CARTESIAN_POINT('Ctrl Pts',(34.8891360058222,-72.9038685237575,-26.9446160351915));
#27966=CARTESIAN_POINT('Ctrl Pts',(34.8782556851746,-72.8990223753931,-26.9459533685205));
#27967=CARTESIAN_POINT('Ctrl Pts',(34.8661901327592,-72.8936483189661,-26.9474363822937));
#27968=CARTESIAN_POINT('Ctrl Pts',(34.8532359023791,-72.8878688487729,-26.9489988385702));
#27969=CARTESIAN_POINT('Ctrl Pts',(34.8395767580721,-72.8817618891628,-26.9506060319683));
#27970=CARTESIAN_POINT('Ctrl Pts',(34.8227985438473,-72.8742604033963,-26.9525802284866));
#27971=CARTESIAN_POINT('Ctrl Pts',(34.8049582468976,-72.8662653078647,-26.9546212264818));
#27972=CARTESIAN_POINT('Ctrl Pts',(34.7864724488064,-72.8579574601953,-26.9566627807048));
#27973=CARTESIAN_POINT('Ctrl Pts',(34.7675828912716,-72.8494681558239,-26.9587489257425));
#27974=CARTESIAN_POINT('Ctrl Pts',(34.7480248947017,-72.8406547386309,-26.9608347976192));
#27975=CARTESIAN_POINT('Ctrl Pts',(34.7282533823277,-72.8317188036679,-26.9628611127832));
#27976=CARTESIAN_POINT('Ctrl Pts',(34.7124762273523,-72.8245881589253,-26.9644780598212));
#27977=CARTESIAN_POINT('Ctrl Pts',(34.696564433511,-72.8173801925988,-26.9660572643433));
#27978=CARTESIAN_POINT('Ctrl Pts',(34.6807169754739,-72.8101846360259,-26.9675781040795));
#27979=CARTESIAN_POINT('Ctrl Pts',(34.6665630018486,-72.8037580080004,-26.9689364244778));
#27980=CARTESIAN_POINT('Ctrl Pts',(34.6524608371956,-72.7973415389273,-26.97024828839));
#27981=CARTESIAN_POINT('Ctrl Pts',(34.6385132007751,-72.7909823722005,-26.9715057794887));
#27982=CARTESIAN_POINT('Ctrl Pts',(34.6255150592532,-72.7850561101023,-26.9726776660199));
#27983=CARTESIAN_POINT('Ctrl Pts',(34.6126514510974,-72.7791797850873,-26.9738024027868));
#27984=CARTESIAN_POINT('Ctrl Pts',(34.5999640381744,-72.7733731934708,-26.9748786719902));
#27985=CARTESIAN_POINT('Ctrl Pts',(34.5879150073292,-72.7678587673291,-26.9759007874449));
#27986=CARTESIAN_POINT('Ctrl Pts',(34.5760251336394,-72.7624073601635,-26.9768792489179));
#27987=CARTESIAN_POINT('Ctrl Pts',(34.5642872567015,-72.7570166655066,-26.9778167794594));
#27988=CARTESIAN_POINT('Ctrl Pts',(34.5530188709448,-72.7518415876615,-26.9787168106879));
#27989=CARTESIAN_POINT('Ctrl Pts',(34.5418907636116,-72.7467225624016,-26.9795791705311));
#27990=CARTESIAN_POINT('Ctrl Pts',(34.5308528639428,-72.7416377007136,-26.9804091399319));
#27991=CARTESIAN_POINT('Ctrl Pts',(34.5195158985983,-72.7364150675617,-26.9812615968862));
#27992=CARTESIAN_POINT('Ctrl Pts',(34.5082747656363,-72.7312287891322,-26.9820799238305));
#27993=CARTESIAN_POINT('Ctrl Pts',(34.4970205175406,-72.7260301710798,-26.9828723349505));
#27994=CARTESIAN_POINT('Ctrl Pts',(34.4862852692864,-72.7210712920061,-26.9836282033142));
#27995=CARTESIAN_POINT('Ctrl Pts',(34.4755303076514,-72.7160976402511,-26.9843609983882));
#27996=CARTESIAN_POINT('Ctrl Pts',(34.4646732598926,-72.7110723522028,-26.9850752378703));
#27997=CARTESIAN_POINT('Ctrl Pts',(34.4534286993624,-72.7058677001745,-26.9858149701869));
#27998=CARTESIAN_POINT('Ctrl Pts',(34.4420748272551,-72.7006077369017,-26.9865347189658));
#27999=CARTESIAN_POINT('Ctrl Pts',(34.430570481744,-72.6952744058455,-26.9872349869545));
#28000=CARTESIAN_POINT('Ctrl Pts',(34.4182666858938,-72.6895704554162,-26.9879839173797));
#28001=CARTESIAN_POINT('Ctrl Pts',(34.4057908222855,-72.6837825957362,-26.988710478766));
#28002=CARTESIAN_POINT('Ctrl Pts',(34.3931476618623,-72.677913979816,-26.9894114998166));
#28003=CARTESIAN_POINT('Ctrl Pts',(34.3797343823661,-72.6716878952801,-26.9901552213997));
#28004=CARTESIAN_POINT('Ctrl Pts',(34.3661331323945,-72.6653710565065,-26.9908700643537));
#28005=CARTESIAN_POINT('Ctrl Pts',(34.3524066390149,-72.6589935209781,-26.9915498852828));
#28006=CARTESIAN_POINT('Ctrl Pts',(34.3374926243335,-72.6520642451703,-26.9922885196183));
#28007=CARTESIAN_POINT('Ctrl Pts',(34.3224312497526,-72.6450635337418,-26.9929856248129));
#28008=CARTESIAN_POINT('Ctrl Pts',(34.3073622391497,-72.6380574390556,-26.9936332024702));
#28009=CARTESIAN_POINT('Ctrl Pts',(34.2898834604621,-72.6299309613649,-26.9943843378204));
#28010=CARTESIAN_POINT('Ctrl Pts',(34.2723953226409,-72.6217976616031,-26.995068492125));
#28011=CARTESIAN_POINT('Ctrl Pts',(34.2551825307308,-72.6137916939583,-26.9956775890499));
#28012=CARTESIAN_POINT('Ctrl Pts',(34.2331249689417,-72.6035323399309,-26.9964581244288));
#28013=CARTESIAN_POINT('Ctrl Pts',(34.2115248288828,-72.5934845725505,-26.9971144521715));
#28014=CARTESIAN_POINT('Ctrl Pts',(34.1910392653848,-72.5839576125602,-26.9976485299606));
#28015=CARTESIAN_POINT('Ctrl Pts',(34.1763977434987,-72.5771484665379,-26.9980302481222));
#28016=CARTESIAN_POINT('Ctrl Pts',(34.1623275344883,-72.5706062766722,-26.9983500673599));
#28017=CARTESIAN_POINT('Ctrl Pts',(34.1490472500448,-72.5644337382725,-26.998615458806));
#28018=CARTESIAN_POINT('Ctrl Pts',(34.1371264940464,-72.5588930945864,-26.9988536816156));
#28019=CARTESIAN_POINT('Ctrl Pts',(34.1258429051091,-72.5536506163926,-26.999048201826));
#28020=CARTESIAN_POINT('Ctrl Pts',(34.1153205042047,-72.5487644340835,-26.9992071337772));
#28021=CARTESIAN_POINT('Ctrl Pts',(34.1054956763343,-72.5442021768033,-26.9993555294788));
#28022=CARTESIAN_POINT('Ctrl Pts',(34.0963348925316,-72.5399507407317,-26.9994729902421));
#28023=CARTESIAN_POINT('Ctrl Pts',(34.0879000947392,-72.5360390514954,-26.9995669997594));
#28024=CARTESIAN_POINT('Ctrl Pts',(34.0798812223448,-72.5323202502147,-26.9996563736059));
#28025=CARTESIAN_POINT('Ctrl Pts',(34.0725188196205,-72.5289086594304,-26.9997246070626));
#28026=CARTESIAN_POINT('Ctrl Pts',(34.0658243155296,-72.5258095023092,-26.9997779400933));
#28027=CARTESIAN_POINT('Ctrl Pts',(34.0593930548309,-72.5228322112176,-26.9998291759458));
#28028=CARTESIAN_POINT('Ctrl Pts',(34.0535784467592,-72.5201433779336,-26.9998666884134));
#28029=CARTESIAN_POINT('Ctrl Pts',(34.0483470066375,-72.5177272092184,-26.9998952450266));
#28030=CARTESIAN_POINT('Ctrl Pts',(34.0433636057174,-72.5154255987405,-26.99992244768));
#28031=CARTESIAN_POINT('Ctrl Pts',(34.038909464426,-72.5133714448828,-26.9999415292289));
#28032=CARTESIAN_POINT('Ctrl Pts',(34.0349130827146,-72.5115312156494,-26.999955676367));
#28033=CARTESIAN_POINT('Ctrl Pts',(34.0310069639009,-72.5097325501193,-26.9999695039757));
#28034=CARTESIAN_POINT('Ctrl Pts',(34.027538362589,-72.5081383474965,-26.9999786149847));
#28035=CARTESIAN_POINT('Ctrl Pts',(34.0243965595917,-72.506696796225,-26.999985050899));
#28036=CARTESIAN_POINT('Ctrl Pts',(34.0213534678907,-72.5053005365886,-26.9999912846053));
#28037=CARTESIAN_POINT('Ctrl Pts',(34.0186170471667,-72.5040475253501,-26.9999950010979));
#28038=CARTESIAN_POINT('Ctrl Pts',(34.0160430187993,-72.5028703359362,-26.9999972537214));
#28039=CARTESIAN_POINT('Ctrl Pts',(34.0138720346514,-72.5018774721476,-26.9999991536266));
#28040=CARTESIAN_POINT('Ctrl Pts',(34.0118159287574,-72.5009382459881,-27.));
#28041=CARTESIAN_POINT('Ctrl Pts',(34.0097619285762,-72.5,-27.));
#28042=CARTESIAN_POINT('',(38.6706975330488,-74.,-25.4999999993376));
#28043=CARTESIAN_POINT('Ctrl Pts',(38.670697532745,-74.,-25.4999999988754));
#28044=CARTESIAN_POINT('Ctrl Pts',(38.3641779127485,-74.0000000001514,-25.7018870729982));
#28045=CARTESIAN_POINT('Ctrl Pts',(37.5431082034452,-73.8929551961393,-26.1757552250324));
#28046=CARTESIAN_POINT('Ctrl Pts',(36.7538439760921,-73.6459407607355,-26.4950027398036));
#28047=CARTESIAN_POINT('Ctrl Pts',(35.7977539931684,-73.2955896700455,-26.7874092748223));
#28048=CARTESIAN_POINT('Ctrl Pts',(35.3787212463313,-73.1202082882644,-26.8774051537635));
#28049=CARTESIAN_POINT('Ctrl Pts',(34.9928690003034,-72.9498135639887,-26.9309674201923));
#28050=CARTESIAN_POINT('',(5.2,-74.,-25.5));
#28051=CARTESIAN_POINT('Origin',(-4.79999999999999,-32.,-20.));
#28052=CARTESIAN_POINT('',(-11.8,-32.,-20.));
#28053=CARTESIAN_POINT('Ctrl Pts',(-11.7309675556501,-72.9498131330638,
19.7928680244678));
#28054=CARTESIAN_POINT('Ctrl Pts',(-11.731923849979,-72.9467709227377,19.7859790576247));
#28055=CARTESIAN_POINT('Ctrl Pts',(-11.7337973388594,-72.9403543075767,
19.7715236532945));
#28056=CARTESIAN_POINT('Ctrl Pts',(-11.745649829374,-72.9035149361054,19.6878044517073));
#28057=CARTESIAN_POINT('Ctrl Pts',(-11.7734458065936,-72.7907458667152,
19.4364960250678));
#28058=CARTESIAN_POINT('Ctrl Pts',(-11.7924941021948,-72.6655779568151,
19.1664451757454));
#28059=CARTESIAN_POINT('Ctrl Pts',(-11.8001369161947,-72.5485936434818,
18.9151456492252));
#28060=CARTESIAN_POINT('Ctrl Pts',(-11.7998430894499,-72.5097905790976,
18.8311911012471));
#28061=CARTESIAN_POINT('Ctrl Pts',(-11.8,-72.5031610690666,18.8166823681909));
#28062=CARTESIAN_POINT('Ctrl Pts',(-11.8,-72.5,18.8097619285762));
#28063=CARTESIAN_POINT('Ctrl Pts',(-11.7529186757946,-72.648770667648,19.9322264436722));
#28064=CARTESIAN_POINT('Ctrl Pts',(-11.7533741068931,-72.646492978889,19.9271259487491));
#28065=CARTESIAN_POINT('Ctrl Pts',(-11.7541650463145,-72.6424667118156,
19.9181034609183));
#28066=CARTESIAN_POINT('Ctrl Pts',(-11.7623844804504,-72.6172317023529,
19.8602296711434));
#28067=CARTESIAN_POINT('Ctrl Pts',(-11.7851097685095,-72.5287894228312,
19.6622836986296));
#28068=CARTESIAN_POINT('Ctrl Pts',(-11.7974871269408,-72.4421791346063,
19.4764698099938));
#28069=CARTESIAN_POINT('Ctrl Pts',(-11.8015614206973,-72.3497074879145,
19.2786156236357));
#28070=CARTESIAN_POINT('Ctrl Pts',(-11.79999556323,-72.3228009293553,19.2206367739928));
#28071=CARTESIAN_POINT('Ctrl Pts',(-11.8,-72.3186768516068,19.2116122804521));
#28072=CARTESIAN_POINT('Ctrl Pts',(-11.8,-72.3163422783269,19.2065079523841));
#28073=CARTESIAN_POINT('Ctrl Pts',(-11.7748697959391,-72.3477282022321,
20.0715848628766));
#28074=CARTESIAN_POINT('Ctrl Pts',(-11.7750197265738,-72.3462456838324,
20.0683082748074));
#28075=CARTESIAN_POINT('Ctrl Pts',(-11.7755924033863,-72.3423623378614,
20.0597599762898));
#28076=CARTESIAN_POINT('Ctrl Pts',(-11.7789296771626,-72.3223173268409,
20.0158887345708));
#28077=CARTESIAN_POINT('Ctrl Pts',(-11.7857195676337,-72.2729882610716,
19.9084439154536));
#28078=CARTESIAN_POINT('Ctrl Pts',(-11.7947091257581,-72.207684036952,19.7662748679286));
#28079=CARTESIAN_POINT('Ctrl Pts',(-11.7983929922402,-72.1582937366765,
19.6589744106553));
#28080=CARTESIAN_POINT('Ctrl Pts',(-11.7997584237843,-72.1381225473783,
19.6151072341032));
#28081=CARTESIAN_POINT('Ctrl Pts',(-11.8,-72.134192634147,19.6065421927134));
#28082=CARTESIAN_POINT('Ctrl Pts',(-11.8,-72.1326845566538,19.6032539761921));
#28083=CARTESIAN_POINT('Ctrl Pts',(-11.7968209160836,-72.0466857368163,
20.210943282081));
#28084=CARTESIAN_POINT('Ctrl Pts',(-11.7968652729023,-72.0460043569062,
20.2094720016796));
#28085=CARTESIAN_POINT('Ctrl Pts',(-11.7969519847552,-72.044574118995,20.2063835827652));
#28086=CARTESIAN_POINT('Ctrl Pts',(-11.7975053588681,-72.0362657186926,
20.1884442076621));
#28087=CARTESIAN_POINT('Ctrl Pts',(-11.7987930795194,-72.0112738645727,
20.1344718117455));
#28088=CARTESIAN_POINT('Ctrl Pts',(-11.7996559734539,-71.9844301297503,
20.0764810684143));
#28089=CARTESIAN_POINT('Ctrl Pts',(-11.8000061189177,-71.9594531450371,
20.0225217914491));
#28090=CARTESIAN_POINT('Ctrl Pts',(-11.7999927847675,-71.9511381222097,
20.004560057106));
#28091=CARTESIAN_POINT('Ctrl Pts',(-11.8,-71.9497084166872,20.0014721049746));
#28092=CARTESIAN_POINT('Ctrl Pts',(-11.8,-71.9490268349807,20.));
#28093=CARTESIAN_POINT('',(-11.8,-72.5,18.8097619285762));
#28094=CARTESIAN_POINT('',(-11.7309675556501,-72.9498131330638,19.7928680244678));
#28095=CARTESIAN_POINT('Ctrl Pts',(-11.8,-72.5,18.8097619285762));
#28096=CARTESIAN_POINT('Ctrl Pts',(-11.8,-72.501104434069,18.8121798350255));
#28097=CARTESIAN_POINT('Ctrl Pts',(-11.799998844824,-72.5022107400032,18.8146017627203));
#28098=CARTESIAN_POINT('Ctrl Pts',(-11.7999961395225,-72.5034031482093,
18.8172080904455));
#28099=CARTESIAN_POINT('Ctrl Pts',(-11.7999933680139,-72.5046247382961,
18.8198782029923));
#28100=CARTESIAN_POINT('Ctrl Pts',(-11.7999889720745,-72.5059366396841,
18.8227417275941));
#28101=CARTESIAN_POINT('Ctrl Pts',(-11.7999817153247,-72.5074063278034,
18.8259430216939));
#28102=CARTESIAN_POINT('Ctrl Pts',(-11.7999742566232,-72.5089169166044,
18.8292334061994));
#28103=CARTESIAN_POINT('Ctrl Pts',(-11.7999637834255,-72.5105941315299,
18.83288047915));
#28104=CARTESIAN_POINT('Ctrl Pts',(-11.7999480152244,-72.5124880592726,
18.8369912426304));
#28105=CARTESIAN_POINT('Ctrl Pts',(-11.799931738317,-72.5144430880226,18.8412346256316));
#28106=CARTESIAN_POINT('Ctrl Pts',(-11.7999098218899,-72.5166289622411,
18.8459719331802));
#28107=CARTESIAN_POINT('Ctrl Pts',(-11.7998786784034,-72.5190774754851,
18.8512709182692));
#28108=CARTESIAN_POINT('Ctrl Pts',(-11.7998456108804,-72.5216772572391,
18.856897273276));
#28109=CARTESIAN_POINT('Ctrl Pts',(-11.7998021319534,-72.5245731226337,
18.8631568226208));
#28110=CARTESIAN_POINT('Ctrl Pts',(-11.7997427762118,-72.5277777824963,
18.8700764316877));
#28111=CARTESIAN_POINT('Ctrl Pts',(-11.7996802900758,-72.5311514546459,
18.8773609777534));
#28112=CARTESIAN_POINT('Ctrl Pts',(-11.7996001669453,-72.5348672363336,
18.8853767852421));
#28113=CARTESIAN_POINT('Ctrl Pts',(-11.7994951564366,-72.5389136971142,
18.8940991505868));
#28114=CARTESIAN_POINT('Ctrl Pts',(-11.7993826824823,-72.5432477533008,
18.9034414434036));
#28115=CARTESIAN_POINT('Ctrl Pts',(-11.7992415706987,-72.5479610044147,
18.9135939447027));
#28116=CARTESIAN_POINT('Ctrl Pts',(-11.7990629471554,-72.5530120784887,
18.9244681723169));
#28117=CARTESIAN_POINT('Ctrl Pts',(-11.7988649429092,-72.558611195469,18.936522256575));
#28118=CARTESIAN_POINT('Ctrl Pts',(-11.7986206702861,-72.5646251589742,
18.9494626076275));
#28119=CARTESIAN_POINT('Ctrl Pts',(-11.7983202304374,-72.57096821163,18.9631064122645));
#28120=CARTESIAN_POINT('Ctrl Pts',(-11.7979524431966,-72.5787331397677,
18.9798086482823));
#28121=CARTESIAN_POINT('Ctrl Pts',(-11.7974999722516,-72.5869905301776,
18.9975635488976));
#28122=CARTESIAN_POINT('Ctrl Pts',(-11.7969538016201,-72.5955474532106,
19.0159607182475));
#28123=CARTESIAN_POINT('Ctrl Pts',(-11.7963926885023,-72.6043384820302,
19.0348612091517));
#28124=CARTESIAN_POINT('Ctrl Pts',(-11.7957325786725,-72.6134430509656,
19.0544340658146));
#28125=CARTESIAN_POINT('Ctrl Pts',(-11.7949775407195,-72.6226464542671,
19.0742232187693));
#28126=CARTESIAN_POINT('Ctrl Pts',(-11.7943746852057,-72.629994856297,19.0900237489622));
#28127=CARTESIAN_POINT('Ctrl Pts',(-11.7937117025217,-72.6374056335299,
19.1059608261794));
#28128=CARTESIAN_POINT('Ctrl Pts',(-11.7929961401608,-72.6447844102966,
19.1218342983521));
#28129=CARTESIAN_POINT('Ctrl Pts',(-11.792357485478,-72.6513701260821,19.136001711131));
#28130=CARTESIAN_POINT('Ctrl Pts',(-11.7916771251311,-72.6579301278489,
19.1501179668206));
#28131=CARTESIAN_POINT('Ctrl Pts',(-11.7909619574117,-72.6644154541125,
19.1640797110818));
#28132=CARTESIAN_POINT('Ctrl Pts',(-11.7902956522372,-72.6704576821541,
19.1770875443434));
#28133=CARTESIAN_POINT('Ctrl Pts',(-11.7895992563685,-72.6764349461207,
19.1899609298704));
#28134=CARTESIAN_POINT('Ctrl Pts',(-11.7888777417671,-72.6823268221364,
19.2026576733767));
#28135=CARTESIAN_POINT('Ctrl Pts',(-11.7881926293819,-72.6879214382716,
19.2147138344186));
#28136=CARTESIAN_POINT('Ctrl Pts',(-11.7874849648868,-72.6934389605026,
19.226610481107));
#28137=CARTESIAN_POINT('Ctrl Pts',(-11.7867569121391,-72.6988815833769,
19.2383542485831));
#28138=CARTESIAN_POINT('Ctrl Pts',(-11.7860580430633,-72.7041060411245,
19.2496272723425));
#28139=CARTESIAN_POINT('Ctrl Pts',(-11.7853404669398,-72.7092614026539,
19.2607592299266));
#28140=CARTESIAN_POINT('Ctrl Pts',(-11.7846028726666,-72.7143695651672,
19.2717996399125));
#28141=CARTESIAN_POINT('Ctrl Pts',(-11.783851133165,-72.7195756895665,19.2830517775755));
#28142=CARTESIAN_POINT('Ctrl Pts',(-11.7830787256541,-72.7247325197476,
19.2942082079411));
#28143=CARTESIAN_POINT('Ctrl Pts',(-11.782279253214,-72.7298873974176,19.305374569448));
#28144=CARTESIAN_POINT('Ctrl Pts',(-11.7815108442834,-72.7348419822645,
19.3161070618677));
#28145=CARTESIAN_POINT('Ctrl Pts',(-11.7807168472023,-72.7397983610911,
19.3268566425138));
#28146=CARTESIAN_POINT('Ctrl Pts',(-11.7798905612536,-72.7447936410788,
19.3377066031678));
#28147=CARTESIAN_POINT('Ctrl Pts',(-11.7790348821557,-72.7499666162216,
19.3489425252584));
#28148=CARTESIAN_POINT('Ctrl Pts',(-11.7781445235792,-72.7551812136779,
19.3602859041663));
#28149=CARTESIAN_POINT('Ctrl Pts',(-11.7772145611532,-72.7604556398259,
19.3717788059764));
#28150=CARTESIAN_POINT('Ctrl Pts',(-11.7762202119557,-72.7660952455349,
19.3840674290118));
#28151=CARTESIAN_POINT('Ctrl Pts',(-11.7751805066769,-72.7718032174321,
19.3965269512495));
#28152=CARTESIAN_POINT('Ctrl Pts',(-11.7740933204493,-72.7775768048788,
19.409153596826));
#28153=CARTESIAN_POINT('Ctrl Pts',(-11.7729402752532,-72.7837001415264,
19.4225451323848));
#28154=CARTESIAN_POINT('Ctrl Pts',(-11.7717337402544,-72.7898971149349,
19.4361243256637));
#28155=CARTESIAN_POINT('Ctrl Pts',(-11.7704767177068,-72.7961388570963,
19.4498295830909));
#28156=CARTESIAN_POINT('Ctrl Pts',(-11.7691117732257,-72.8029164853351,
19.4647115082578));
#28157=CARTESIAN_POINT('Ctrl Pts',(-11.7676871916452,-72.8097466432146,
19.479741585126));
#28158=CARTESIAN_POINT('Ctrl Pts',(-11.766214782111,-72.8165662848746,19.4947816596443));
#28159=CARTESIAN_POINT('Ctrl Pts',(-11.7645116079786,-72.8244547404956,
19.51217890224));
#28160=CARTESIAN_POINT('Ctrl Pts',(-11.7627442453546,-72.8323286372044,
19.5295886154485));
#28161=CARTESIAN_POINT('Ctrl Pts',(-11.7609440847192,-72.8400623197651,
19.5467306475706));
#28162=CARTESIAN_POINT('Ctrl Pts',(-11.7585963565591,-72.8501484109567,
19.5690868921974));
#28163=CARTESIAN_POINT('Ctrl Pts',(-11.7561926064093,-72.8599933687506,
19.5909825486672));
#28164=CARTESIAN_POINT('Ctrl Pts',(-11.7538294614589,-72.8692964892794,
19.6117338510281));
#28165=CARTESIAN_POINT('Ctrl Pts',(-11.7521606565975,-72.8758661636289,
19.6263879983561));
#28166=CARTESIAN_POINT('Ctrl Pts',(-11.750512913278,-72.8821649104921,19.6404694774992));
#28167=CARTESIAN_POINT('Ctrl Pts',(-11.7489236489795,-72.8880982600167,
19.6537587709998));
#28168=CARTESIAN_POINT('Ctrl Pts',(-11.7474976601362,-72.8934220379643,
19.6656827689681));
#28169=CARTESIAN_POINT('Ctrl Pts',(-11.746118990168,-72.8984513774563,19.6769682936816));
#28170=CARTESIAN_POINT('Ctrl Pts',(-11.7448124401235,-72.9031339887237,
19.6874909539757));
#28171=CARTESIAN_POINT('Ctrl Pts',(-11.7435926877885,-72.9075055212583,
19.6973145650337));
#28172=CARTESIAN_POINT('Ctrl Pts',(-11.7424359361705,-72.9115747003093,
19.7064728666794));
#28173=CARTESIAN_POINT('Ctrl Pts',(-11.7413577511394,-72.9153165458182,
19.7149037671804));
#28174=CARTESIAN_POINT('Ctrl Pts',(-11.7403328121501,-72.9188736007237,
19.722918308645));
#28175=CARTESIAN_POINT('Ctrl Pts',(-11.7393789657513,-72.9221347341473,
19.7302752031999));
#28176=CARTESIAN_POINT('Ctrl Pts',(-11.7385035999542,-72.925096921794,19.7369630176401));
#28177=CARTESIAN_POINT('Ctrl Pts',(-11.7376626969175,-72.9279424894366,
19.743387535814));
#28178=CARTESIAN_POINT('Ctrl Pts',(-11.7368942766262,-72.9305120885608,
19.7491943710544));
#28179=CARTESIAN_POINT('Ctrl Pts',(-11.7361981280593,-72.9328220615438,
19.7544171202232));
#28180=CARTESIAN_POINT('Ctrl Pts',(-11.7355350110767,-72.935022428516,19.7593920549342));
#28181=CARTESIAN_POINT('Ctrl Pts',(-11.7349374860318,-72.9369871912694,
19.7638369366522));
#28182=CARTESIAN_POINT('Ctrl Pts',(-11.7343986079509,-72.9387489413189,
19.7678234681457));
#28183=CARTESIAN_POINT('Ctrl Pts',(-11.73387191165,-72.940470865567,19.7717198808326));
#28184=CARTESIAN_POINT('Ctrl Pts',(-11.7334012661809,-72.9419987635744,
19.7751782288516));
#28185=CARTESIAN_POINT('Ctrl Pts',(-11.7329732356419,-72.9433821218023,
19.7783095280656));
#28186=CARTESIAN_POINT('Ctrl Pts',(-11.7325586563635,-72.9447220067026,
19.7813424232698));
#28187=CARTESIAN_POINT('Ctrl Pts',(-11.7321840603972,-72.9459262548977,
19.7840684168231));
#28188=CARTESIAN_POINT('Ctrl Pts',(-11.7318304518762,-72.9470587848148,
19.7866321657248));
#28189=CARTESIAN_POINT('Ctrl Pts',(-11.7315331756714,-72.9480108947768,
19.788787491454));
#28190=CARTESIAN_POINT('Ctrl Pts',(-11.7312506313311,-72.948912598852,19.7908287998052));
#28191=CARTESIAN_POINT('Ctrl Pts',(-11.7309675556501,-72.9498131330638,
19.7928680244678));
#28192=CARTESIAN_POINT('',(-11.7968209160836,-72.0466857368163,20.210943282081));
#28193=CARTESIAN_POINT('Ctrl Pts',(-11.7968209160836,-72.0466857368163,
20.210943282081));
#28194=CARTESIAN_POINT('Ctrl Pts',(-11.7748697959391,-72.3477282022321,
20.0715848628766));
#28195=CARTESIAN_POINT('Ctrl Pts',(-11.7529186757946,-72.648770667648,19.9322264436722));
#28196=CARTESIAN_POINT('Ctrl Pts',(-11.7309675556501,-72.9498131330638,
19.7928680244678));
#28197=CARTESIAN_POINT('',(-11.8,-71.9490268349807,20.));
#28198=CARTESIAN_POINT('Ctrl Pts',(-11.7968209160836,-72.0466857368163,
20.210943282081));
#28199=CARTESIAN_POINT('Ctrl Pts',(-11.7968440264343,-72.0463307309993,
20.2101767301277));
#28200=CARTESIAN_POINT('Ctrl Pts',(-11.796867151744,-72.0459737810207,20.2094059772171));
#28201=CARTESIAN_POINT('Ctrl Pts',(-11.7968938349779,-72.0455591055399,
20.2085105801841));
#28202=CARTESIAN_POINT('Ctrl Pts',(-11.7969215748069,-72.0451280098565,
20.2075797274724));
#28203=CARTESIAN_POINT('Ctrl Pts',(-11.7969531556842,-72.0446346198902,
20.2065143654833));
#28204=CARTESIAN_POINT('Ctrl Pts',(-11.7969907706432,-72.0440407131694,
20.2052319554395));
#28205=CARTESIAN_POINT('Ctrl Pts',(-11.7970302352795,-72.0434176016909,
20.2038864841889));
#28206=CARTESIAN_POINT('Ctrl Pts',(-11.7970763351041,-72.0426839627647,
20.2023023485085));
#28207=CARTESIAN_POINT('Ctrl Pts',(-11.7971297471362,-72.0418204588819,
20.2004377752349));
#28208=CARTESIAN_POINT('Ctrl Pts',(-11.7971866204212,-72.0409009974715,
20.1984523722666));
#28209=CARTESIAN_POINT('Ctrl Pts',(-11.7972517663276,-72.039834454825,20.1961493535317));
#28210=CARTESIAN_POINT('Ctrl Pts',(-11.7973241283667,-72.0386228526127,
20.1935330529333));
#28211=CARTESIAN_POINT('Ctrl Pts',(-11.7974033531205,-72.0372963437394,
20.1906686260414));
#28212=CARTESIAN_POINT('Ctrl Pts',(-11.7974911870066,-72.0357962057728,
20.1874292153278));
#28213=CARTESIAN_POINT('Ctrl Pts',(-11.797584514987,-72.0341515121678,20.1838775560358));
#28214=CARTESIAN_POINT('Ctrl Pts',(-11.7976993757062,-72.0321273529657,
20.1795064538339));
#28215=CARTESIAN_POINT('Ctrl Pts',(-11.7978224459019,-72.0298846925149,
20.1746633732519));
#28216=CARTESIAN_POINT('Ctrl Pts',(-11.7979466024095,-72.0275116964433,
20.1695386381506));
#28217=CARTESIAN_POINT('Ctrl Pts',(-11.7980821533145,-72.0249209199172,
20.1639435832067));
#28218=CARTESIAN_POINT('Ctrl Pts',(-11.7982187728114,-72.0221774130801,
20.158018473028));
#28219=CARTESIAN_POINT('Ctrl Pts',(-11.7983487795842,-72.0194065699847,
20.1520340728002));
#28220=CARTESIAN_POINT('Ctrl Pts',(-11.7984473485597,-72.0173057627787,
20.1474967999597));
#28221=CARTESIAN_POINT('Ctrl Pts',(-11.798542156045,-72.0151898308566,20.1429267194323));
#28222=CARTESIAN_POINT('Ctrl Pts',(-11.798631372502,-72.0131013188954,20.1384157210412));
#28223=CARTESIAN_POINT('Ctrl Pts',(-11.7987118838834,-72.0112165883329,
20.1343448721818));
#28224=CARTESIAN_POINT('Ctrl Pts',(-11.7987878612489,-72.0093544513597,
20.1303227080409));
#28225=CARTESIAN_POINT('Ctrl Pts',(-11.798859022311,-72.0075300311517,20.1263819046227));
#28226=CARTESIAN_POINT('Ctrl Pts',(-11.7989256149733,-72.0058227351215,
20.1226940930084));
#28227=CARTESIAN_POINT('Ctrl Pts',(-11.7989880057221,-72.0041486403605,
20.1190779023675));
#28228=CARTESIAN_POINT('Ctrl Pts',(-11.7990467044472,-72.0025022857801,
20.1155215519588));
#28229=CARTESIAN_POINT('Ctrl Pts',(-11.7991060919784,-72.0008366118854,
20.1119234691965));
#28230=CARTESIAN_POINT('Ctrl Pts',(-11.799161711364,-71.9991997282623,20.1083874932517));
#28231=CARTESIAN_POINT('Ctrl Pts',(-11.7992146913247,-71.997562572897,20.1048508690689));
#28232=CARTESIAN_POINT('Ctrl Pts',(-11.7992663579433,-71.9959660016519,
20.1014019157228));
#28233=CARTESIAN_POINT('Ctrl Pts',(-11.79931563984,-71.9943651666199,20.0979436948263));
#28234=CARTESIAN_POINT('Ctrl Pts',(-11.7993631272831,-71.9927356970362,
20.0944235798376));
#28235=CARTESIAN_POINT('Ctrl Pts',(-11.7994134018494,-71.991010590962,20.090696862991));
#28236=CARTESIAN_POINT('Ctrl Pts',(-11.7994616361791,-71.9892535447088,
20.0869011062902));
#28237=CARTESIAN_POINT('Ctrl Pts',(-11.7995075723881,-71.987460970195,20.0830285738881));
#28238=CARTESIAN_POINT('Ctrl Pts',(-11.7995572904833,-71.9855208146535,
20.0788372194189));
#28239=CARTESIAN_POINT('Ctrl Pts',(-11.7996042772797,-71.9835392694514,
20.0745564223789));
#28240=CARTESIAN_POINT('Ctrl Pts',(-11.7996476627856,-71.9815377443596,
20.0702324487684));
#28241=CARTESIAN_POINT('Ctrl Pts',(-11.7996984016496,-71.9791969831453,
20.0651756099806));
#28242=CARTESIAN_POINT('Ctrl Pts',(-11.7997441440131,-71.9768292652326,
20.0600605172037));
#28243=CARTESIAN_POINT('Ctrl Pts',(-11.7997837204606,-71.9744988699031,
20.0550260554206));
#28244=CARTESIAN_POINT('Ctrl Pts',(-11.799841617981,-71.9710896677201,20.0476609968471));
#28245=CARTESIAN_POINT('Ctrl Pts',(-11.7998859839155,-71.967763829697,20.0404760377697));
#28246=CARTESIAN_POINT('Ctrl Pts',(-11.799917487043,-71.9647604963972,20.0339878594497));
#28247=CARTESIAN_POINT('Ctrl Pts',(-11.7999376069614,-71.9628423750572,
20.0298440924912));
#28248=CARTESIAN_POINT('Ctrl Pts',(-11.7999526242593,-71.9610565580338,
20.0259861725226));
#28249=CARTESIAN_POINT('Ctrl Pts',(-11.7999637788496,-71.9594514906785,
20.0225187653674));
#28250=CARTESIAN_POINT('Ctrl Pts',(-11.7999740893287,-71.9579678850111,
20.0193137503941));
#28251=CARTESIAN_POINT('Ctrl Pts',(-11.7999811326703,-71.9566391654818,
20.0164433694765));
#28252=CARTESIAN_POINT('Ctrl Pts',(-11.7999861098761,-71.9554826093196,
20.013944946831));
#28253=CARTESIAN_POINT('Ctrl Pts',(-11.7999904546681,-71.9544730074948,
20.0117639787601));
#28254=CARTESIAN_POINT('Ctrl Pts',(-11.7999932364772,-71.9535945583468,
20.0098663653902));
#28255=CARTESIAN_POINT('Ctrl Pts',(-11.7999951540824,-71.9528401206129,
20.0082366754872));
#28256=CARTESIAN_POINT('Ctrl Pts',(-11.7999969972036,-71.952114986876,20.006670286273));
#28257=CARTESIAN_POINT('Ctrl Pts',(-11.7999980448829,-71.9515045768435,
20.0053517545772));
#28258=CARTESIAN_POINT('Ctrl Pts',(-11.7999987249728,-71.9509829203972,
20.0042249709247));
#28259=CARTESIAN_POINT('Ctrl Pts',(-11.7999993730205,-71.9504858415435,
20.0031512751423));
#28260=CARTESIAN_POINT('Ctrl Pts',(-11.7999996854038,-71.9500694193736,
20.0022518343659));
#28261=CARTESIAN_POINT('Ctrl Pts',(-11.7999998528112,-71.9496914618382,
20.0014354939551));
#28262=CARTESIAN_POINT('Ctrl Pts',(-11.7999999551045,-71.9494605131145,
20.0009366739598));
#28263=CARTESIAN_POINT('Ctrl Pts',(-11.8,-71.9492435363226,20.0004680394447));
#28264=CARTESIAN_POINT('Ctrl Pts',(-11.8,-71.9490268349807,20.));
#28265=CARTESIAN_POINT('',(-11.8,-72.2245134174903,19.4048809642881));
#28266=CARTESIAN_POINT('Ctrl Pts',(-5.01094426619173,-72.0466861925674,
26.9968208864141));
#28267=CARTESIAN_POINT('Ctrl Pts',(-5.00947297646683,-72.0460048083194,
26.996865243721));
#28268=CARTESIAN_POINT('Ctrl Pts',(-5.0063845384978,-72.0445745615206,26.9969519565246));
#28269=CARTESIAN_POINT('Ctrl Pts',(-4.98844507070461,-72.0362661183909,
26.9975053360185));
#28270=CARTESIAN_POINT('Ctrl Pts',(-4.93447244718678,-72.0112741569711,
26.9987930679778));
#28271=CARTESIAN_POINT('Ctrl Pts',(-4.87648146296461,-71.984430300943,26.9996559698239));
#28272=CARTESIAN_POINT('Ctrl Pts',(-4.82252191221301,-71.9594531916436,
27.0000061189759));
#28273=CARTESIAN_POINT('Ctrl Pts',(-4.80456008230516,-71.951138130719,26.9999927846913));
#28274=CARTESIAN_POINT('Ctrl Pts',(-4.80147211312516,-71.9497084193948,
27.));
#28275=CARTESIAN_POINT('Ctrl Pts',(-4.8,-71.9490268349807,27.));
#28276=CARTESIAN_POINT('Ctrl Pts',(-4.87158584422818,-72.3477286497075,
26.974869731007));
#28277=CARTESIAN_POINT('Ctrl Pts',(-4.86830922557782,-72.3462461176065,
26.9750196643687));
#28278=CARTESIAN_POINT('Ctrl Pts',(-4.85975897842875,-72.3423627521791,
26.9755114207066));
#28279=CARTESIAN_POINT('Ctrl Pts',(-4.81591321368326,-72.3223177067783,
26.9782702084194));
#28280=CARTESIAN_POINT('Ctrl Pts',(-4.70857333101532,-72.272988635298,26.9845161337709));
#28281=CARTESIAN_POINT('Ctrl Pts',(-4.56639009565372,-72.2076844178794,
26.9930985489782));
#28282=CARTESIAN_POINT('Ctrl Pts',(-4.45903094371778,-72.1582940094813,
26.9980897400517));
#28283=CARTESIAN_POINT('Ctrl Pts',(-4.41511199664308,-72.138122656842,26.9997839104599));
#28284=CARTESIAN_POINT('Ctrl Pts',(-4.40654219803927,-72.1341926745702,
27.));
#28285=CARTESIAN_POINT('Ctrl Pts',(-4.40325397619206,-72.1326845566538,
27.));
#28286=CARTESIAN_POINT('Ctrl Pts',(-4.73222742226463,-72.6487711068476,
26.9529185755998));
#28287=CARTESIAN_POINT('Ctrl Pts',(-4.72712687588195,-72.646493395594,26.9533740167535));
#28288=CARTESIAN_POINT('Ctrl Pts',(-4.71810428296693,-72.6425801839039,
26.9544902505489));
#28289=CARTESIAN_POINT('Ctrl Pts',(-4.66023026081951,-72.6159497943818,
26.962298209812));
#28290=CARTESIAN_POINT('Ctrl Pts',(-4.46228446583122,-72.5231679093969,
26.9782325012995));
#28291=CARTESIAN_POINT('Ctrl Pts',(-4.2764703099712,-72.4384023248246,26.9937562016165));
#28292=CARTESIAN_POINT('Ctrl Pts',(-4.07861571985972,-72.3480976161143,
26.9979643889596));
#28293=CARTESIAN_POINT('Ctrl Pts',(-4.02063678651915,-72.3226743264951,
26.9994070919264));
#28294=CARTESIAN_POINT('Ctrl Pts',(-4.01161228295339,-72.3186769297456,
27.));
#28295=CARTESIAN_POINT('Ctrl Pts',(-4.00650795238413,-72.3163422783269,
27.));
#28296=CARTESIAN_POINT('Ctrl Pts',(-4.59286900030108,-72.9498135639877,
26.9309674201926));
#28297=CARTESIAN_POINT('Ctrl Pts',(-4.5859799608391,-72.9467713218037,26.9319237255424));
#28298=CARTESIAN_POINT('Ctrl Pts',(-4.57152441475369,-72.9403546462486,
26.933797234493));
#28299=CARTESIAN_POINT('Ctrl Pts',(-4.48780490143884,-72.9035150752116,
26.9456497972286));
#28300=CARTESIAN_POINT('Ctrl Pts',(-4.23649663915558,-72.7907461114549,
26.9734457309761));
#28301=CARTESIAN_POINT('Ctrl Pts',(-3.96644557228501,-72.665579292086,26.9924939338067));
#28302=CARTESIAN_POINT('Ctrl Pts',(-3.71514570094186,-72.5485946771508,
27.0001369006243));
#28303=CARTESIAN_POINT('Ctrl Pts',(-3.63119110304352,-72.5097909222079,
26.9998430866664));
#28304=CARTESIAN_POINT('Ctrl Pts',(-3.6166823678675,-72.503161184921,27.));
#28305=CARTESIAN_POINT('Ctrl Pts',(-3.60976192857619,-72.5,27.));
#28306=CARTESIAN_POINT('',(-4.8,-71.9490268349807,27.));
#28307=CARTESIAN_POINT('',(-5.01094426619173,-72.0466861925674,26.9968208864141));
#28308=CARTESIAN_POINT('Ctrl Pts',(-4.8,-71.9490268349807,27.));
#28309=CARTESIAN_POINT('Ctrl Pts',(-4.80076697070348,-71.9493819403517,
27.));
#28310=CARTESIAN_POINT('Ctrl Pts',(-4.80153814101389,-71.9497389896615,
26.9999998883361));
#28311=CARTESIAN_POINT('Ctrl Pts',(-4.80243401101288,-71.9501537584991,
26.9999995768279));
#28312=CARTESIAN_POINT('Ctrl Pts',(-4.8033653543852,-71.9505849507574,26.999999252985));
#28313=CARTESIAN_POINT('Ctrl Pts',(-4.80443126675711,-71.9510784307137,
26.999998715007));
#28314=CARTESIAN_POINT('Ctrl Pts',(-4.80571431921969,-71.9516724170336,
26.9999976676107));
#28315=CARTESIAN_POINT('Ctrl Pts',(-4.80706046220201,-71.9522956109712,
26.9999965687117));
#28316=CARTESIAN_POINT('Ctrl Pts',(-4.80864537002902,-71.9530293205579,
26.9999949098187));
#28317=CARTESIAN_POINT('Ctrl Pts',(-4.81051081979623,-71.953892881673,26.9999921087575));
#28318=CARTESIAN_POINT('Ctrl Pts',(-4.81249715032639,-71.9548124013714,
26.9999891261881));
#28319=CARTESIAN_POINT('Ctrl Pts',(-4.81480121272597,-71.9558789862512,
26.9999848410617));
#28320=CARTESIAN_POINT('Ctrl Pts',(-4.81741864449946,-71.9570906156706,
26.9999783278824));
#28321=CARTESIAN_POINT('Ctrl Pts',(-4.82028429268157,-71.958417146386,26.9999711970451));
#28322=CARTESIAN_POINT('Ctrl Pts',(-4.82352502414162,-71.9599172861368,
26.9999613711321));
#28323=CARTESIAN_POINT('Ctrl Pts',(-4.82707803879157,-71.9615619664985,
26.9999476269337));
#28324=CARTESIAN_POINT('Ctrl Pts',(-4.83145062144543,-71.9635860225549,
26.9999307123839));
#28325=CARTESIAN_POINT('Ctrl Pts',(-4.83629519151344,-71.9658285383687,
26.9999077806186));
#28326=CARTESIAN_POINT('Ctrl Pts',(-4.84142131794206,-71.9682013731942,
26.9998774471001));
#28327=CARTESIAN_POINT('Ctrl Pts',(-4.84701870318713,-71.9707923492121,
26.9998443249382));
#28328=CARTESIAN_POINT('Ctrl Pts',(-4.85294611909829,-71.9735360807744,
26.9998023221268));
#28329=CARTESIAN_POINT('Ctrl Pts',(-4.85893259038397,-71.9763071508735,
26.9997519205891));
#28330=CARTESIAN_POINT('Ctrl Pts',(-4.86347111047887,-71.9784079806827,
26.9997137096998));
#28331=CARTESIAN_POINT('Ctrl Pts',(-4.86804230004885,-71.9805239342998,
26.9996707497673));
#28332=CARTESIAN_POINT('Ctrl Pts',(-4.87255423493374,-71.9826124675569,
26.9996239815431));
#28333=CARTESIAN_POINT('Ctrl Pts',(-4.87662590506207,-71.9844972062981,
26.9995817768601));
#28334=CARTESIAN_POINT('Ctrl Pts',(-4.88064875130215,-71.9863593514082,
26.9995365071788));
#28335=CARTESIAN_POINT('Ctrl Pts',(-4.88459008953543,-71.9881837792468,
26.9994888753931));
#28336=CARTESIAN_POINT('Ctrl Pts',(-4.88827839296645,-71.9898910784073,
26.9994443015788));
#28337=CARTESIAN_POINT('Ctrl Pts',(-4.89189494739972,-71.9915651760262,
26.9993976862506));
#28338=CARTESIAN_POINT('Ctrl Pts',(-4.89545153213979,-71.9932115313249,
26.9993491843894));
#28339=CARTESIAN_POINT('Ctrl Pts',(-4.8990489039423,-71.9948767670949,26.9993001263068));
#28340=CARTESIAN_POINT('Ctrl Pts',(-4.902584072253,-71.9965132267009,26.9992491748664));
#28341=CARTESIAN_POINT('Ctrl Pts',(-4.90611972984301,-71.9981499419667,
26.9991955682734));
#28342=CARTESIAN_POINT('Ctrl Pts',(-4.90956865163276,-71.9997465057742,
26.9991432767429));
#28343=CARTESIAN_POINT('Ctrl Pts',(-4.91302668987658,-72.0013473181756,
26.9990883234737));
#28344=CARTESIAN_POINT('Ctrl Pts',(-4.91654648739712,-72.002976758872,26.999029712487));
#28345=CARTESIAN_POINT('Ctrl Pts',(-4.92027284370588,-72.0047018230506,
26.9989676619233));
#28346=CARTESIAN_POINT('Ctrl Pts',(-4.924068087188,-72.0064588199744,26.9989014928217));
#28347=CARTESIAN_POINT('Ctrl Pts',(-4.92793996922138,-72.0082513459319,
26.9988307140747));
#28348=CARTESIAN_POINT('Ctrl Pts',(-4.9321305670819,-72.0101914245235,26.9987541091412));
#28349=CARTESIAN_POINT('Ctrl Pts',(-4.93641044374858,-72.0121728926472,
26.9986720801898));
#28350=CARTESIAN_POINT('Ctrl Pts',(-4.94073336345865,-72.0141743492429,
26.9985851513295));
#28351=CARTESIAN_POINT('Ctrl Pts',(-4.94578880707783,-72.0165149550498,
26.99848349227));
#28352=CARTESIAN_POINT('Ctrl Pts',(-4.95090231692142,-72.0188825276485,
26.9983750851362));
#28353=CARTESIAN_POINT('Ctrl Pts',(-4.95593510268464,-72.021212804208,26.9982629447421));
#28354=CARTESIAN_POINT('Ctrl Pts',(-4.96329866291305,-72.0246222741522,
26.9980988700954));
#28355=CARTESIAN_POINT('Ctrl Pts',(-4.97048187721421,-72.0279484172632,
26.9979266950891));
#28356=CARTESIAN_POINT('Ctrl Pts',(-4.9769682776892,-72.030952030051,26.9977626587854));
#28357=CARTESIAN_POINT('Ctrl Pts',(-4.9811109071306,-72.0328703289307,26.9976578947297));
#28358=CARTESIAN_POINT('Ctrl Pts',(-4.98496767933264,-72.0346563122562,
26.9975566436896));
#28359=CARTESIAN_POINT('Ctrl Pts',(-4.98843399270563,-72.0362615170322,
26.9974632996818));
#28360=CARTESIAN_POINT('Ctrl Pts',(-4.99163799870267,-72.0377452506638,
26.9973770193232));
#28361=CARTESIAN_POINT('Ctrl Pts',(-4.99450741737523,-72.0390740730504,
26.9972975574334));
#28362=CARTESIAN_POINT('Ctrl Pts',(-4.99700496260522,-72.040230697167,26.9972272397507));
#28363=CARTESIAN_POINT('Ctrl Pts',(-4.99918507340499,-72.041240316011,26.997165859345));
#28364=CARTESIAN_POINT('Ctrl Pts',(-5.00108191836741,-72.0421187666742,
26.9971114553097));
#28365=CARTESIAN_POINT('Ctrl Pts',(-5.00271093426901,-72.0428731874743,
26.9970642613262));
#28366=CARTESIAN_POINT('Ctrl Pts',(-5.00427667108349,-72.0435983028148,
26.9970189005919));
#28367=CARTESIAN_POINT('Ctrl Pts',(-5.00559463926482,-72.0442086780512,
26.9969802139162));
#28368=CARTESIAN_POINT('Ctrl Pts',(-5.00672092624159,-72.0447302826953,
26.9969469383906));
#28369=CARTESIAN_POINT('Ctrl Pts',(-5.00779414404587,-72.0452273100093,
26.9969152307644));
#28370=CARTESIAN_POINT('Ctrl Pts',(-5.0086931690725,-72.0456436659006,26.9968884389805));
#28371=CARTESIAN_POINT('Ctrl Pts',(-5.00950910963114,-72.0460215435603,
26.9968640070378));
#28372=CARTESIAN_POINT('Ctrl Pts',(-5.01000782568555,-72.0462525084922,
26.9968490738397));
#28373=CARTESIAN_POINT('Ctrl Pts',(-5.01047634434494,-72.0464694884266,
26.9968349935968));
#28374=CARTESIAN_POINT('Ctrl Pts',(-5.01094426619173,-72.0466861925674,
26.9968208864141));
#28375=CARTESIAN_POINT('',(-4.59286900030108,-72.9498135639877,26.9309674201926));
#28376=CARTESIAN_POINT('Ctrl Pts',(-4.59286900030108,-72.9498135639877,
26.9309674201926));
#28377=CARTESIAN_POINT('Ctrl Pts',(-4.73222742226463,-72.6487711068476,
26.9529185755998));
#28378=CARTESIAN_POINT('Ctrl Pts',(-4.87158584422818,-72.3477286497075,
26.974869731007));
#28379=CARTESIAN_POINT('Ctrl Pts',(-5.01094426619173,-72.0466861925674,
26.9968208864141));
#28380=CARTESIAN_POINT('',(-3.60976192857619,-72.5,27.));
#28381=CARTESIAN_POINT('Ctrl Pts',(-4.59286900030109,-72.9498135639877,
26.9309674201926));
#28382=CARTESIAN_POINT('Ctrl Pts',(-4.5904606339385,-72.948750014594,26.9313017387358));
#28383=CARTESIAN_POINT('Ctrl Pts',(-4.58804823665763,-72.9476843461918,
26.9316354879945));
#28384=CARTESIAN_POINT('Ctrl Pts',(-4.58545108096436,-72.9465370382974,
26.9319932518796));
#28385=CARTESIAN_POINT('Ctrl Pts',(-4.58279030740325,-72.945361626858,26.9323597792652));
#28386=CARTESIAN_POINT('Ctrl Pts',(-4.57993573759051,-72.9441005819349,
26.9327514972647));
#28387=CARTESIAN_POINT('Ctrl Pts',(-4.57674274787858,-72.9426899331027,
26.9331872254278));
#28388=CARTESIAN_POINT('Ctrl Pts',(-4.57346080562075,-72.9412399854263,
26.9336350924116));
#28389=CARTESIAN_POINT('Ctrl Pts',(-4.56982146787799,-72.9396320460181,
26.9341294433979));
#28390=CARTESIAN_POINT('Ctrl Pts',(-4.56571755385512,-72.9378182307471,
26.9346829603872));
#28391=CARTESIAN_POINT('Ctrl Pts',(-4.56148107948029,-72.9359458275064,
26.9352543565052));
#28392=CARTESIAN_POINT('Ctrl Pts',(-4.55674969938714,-72.9338541062472,
26.935888782133));
#28393=CARTESIAN_POINT('Ctrl Pts',(-4.55145557742484,-72.931512042168,26.9365922725199));
#28394=CARTESIAN_POINT('Ctrl Pts',(-4.54583399063082,-72.9290251110787,
26.9373392768952));
#28395=CARTESIAN_POINT('Ctrl Pts',(-4.53957792038129,-72.9262559163629,
26.938164142488));
#28396=CARTESIAN_POINT('Ctrl Pts',(-4.53266052960038,-72.9231908648878,
26.9390654925595));
#28397=CARTESIAN_POINT('Ctrl Pts',(-4.52537764142081,-72.9199638638603,
26.9400144676846));
#28398=CARTESIAN_POINT('Ctrl Pts',(-4.51736195898021,-72.9164090127371,
26.941048150003));
#28399=CARTESIAN_POINT('Ctrl Pts',(-4.50863836855335,-72.9125349423682,
26.9421563442724));
#28400=CARTESIAN_POINT('Ctrl Pts',(-4.49929320103042,-72.9083848350362,
26.9433435000866));
#28401=CARTESIAN_POINT('Ctrl Pts',(-4.48913600582349,-72.9038685237529,
26.9446160351928));
#28402=CARTESIAN_POINT('Ctrl Pts',(-4.47825568517621,-72.8990223753879,
26.9459533685219));
#28403=CARTESIAN_POINT('Ctrl Pts',(-4.46619013276138,-72.8936483189604,
26.9474363822952));
#28404=CARTESIAN_POINT('Ctrl Pts',(-4.45323590238201,-72.8878688487667,
26.9489988385719));
#28405=CARTESIAN_POINT('Ctrl Pts',(-4.43957675807571,-72.881761889156,26.9506060319701));
#28406=CARTESIAN_POINT('Ctrl Pts',(-4.42279854385202,-72.874260403389,26.9525802284885));
#28407=CARTESIAN_POINT('Ctrl Pts',(-4.40495824690347,-72.8662653078568,
26.9546212264838));
#28408=CARTESIAN_POINT('Ctrl Pts',(-4.38647244881348,-72.8579574601868,
26.9566627807069));
#28409=CARTESIAN_POINT('Ctrl Pts',(-4.36758289127922,-72.8494681558146,
26.9587489257447));
#28410=CARTESIAN_POINT('Ctrl Pts',(-4.3480248947097,-72.8406547386207,26.9608347976216));
#28411=CARTESIAN_POINT('Ctrl Pts',(-4.32825338233612,-72.8317188036569,
26.9628611127856));
#28412=CARTESIAN_POINT('Ctrl Pts',(-4.3124762273609,-72.8245881589137,26.9644780598238));
#28413=CARTESIAN_POINT('Ctrl Pts',(-4.29656443351978,-72.8173801925865,
26.966057264346));
#28414=CARTESIAN_POINT('Ctrl Pts',(-4.28071697548282,-72.810184636013,26.9675781040822));
#28415=CARTESIAN_POINT('Ctrl Pts',(-4.26656300185773,-72.8037580079872,
26.9689364244806));
#28416=CARTESIAN_POINT('Ctrl Pts',(-4.25246083720482,-72.7973415389137,
26.9702482883927));
#28417=CARTESIAN_POINT('Ctrl Pts',(-4.23851320078447,-72.7909823721865,
26.9715057794914));
#28418=CARTESIAN_POINT('Ctrl Pts',(-4.22551505926242,-72.785056110088,26.9726776660227));
#28419=CARTESIAN_POINT('Ctrl Pts',(-4.21265145110638,-72.7791797850726,
26.9738024027896));
#28420=CARTESIAN_POINT('Ctrl Pts',(-4.19996403818309,-72.7733731934558,
26.974878671993));
#28421=CARTESIAN_POINT('Ctrl Pts',(-4.187915007338,-72.767858767314,26.9759007874477));
#28422=CARTESIAN_POINT('Ctrl Pts',(-4.17602513364819,-72.7624073601484,
26.9768792489206));
#28423=CARTESIAN_POINT('Ctrl Pts',(-4.16428725671022,-72.7570166654915,
26.9778167794621));
#28424=CARTESIAN_POINT('Ctrl Pts',(-4.15301887095358,-72.7518415876464,
26.9787168106905));
#28425=CARTESIAN_POINT('Ctrl Pts',(-4.14189076362031,-72.7467225623866,
26.9795791705336));
#28426=CARTESIAN_POINT('Ctrl Pts',(-4.13085286395148,-72.7416377006988,
26.9804091399343));
#28427=CARTESIAN_POINT('Ctrl Pts',(-4.11951589860725,-72.7364150675471,
26.9812615968885));
#28428=CARTESIAN_POINT('Ctrl Pts',(-4.10827476564544,-72.731228789118,26.9820799238327));
#28429=CARTESIAN_POINT('Ctrl Pts',(-4.09702051754996,-72.726030171066,26.9828723349526));
#28430=CARTESIAN_POINT('Ctrl Pts',(-4.08628526929532,-72.7210712919924,
26.9836282033163));
#28431=CARTESIAN_POINT('Ctrl Pts',(-4.07553030765988,-72.7160976402375,
26.9843609983902));
#28432=CARTESIAN_POINT('Ctrl Pts',(-4.06467325990052,-72.7110723521894,
26.9850752378722));
#28433=CARTESIAN_POINT('Ctrl Pts',(-4.05342869936957,-72.7058677001612,
26.9858149701888));
#28434=CARTESIAN_POINT('Ctrl Pts',(-4.04207482726141,-72.7006077368884,
26.9865347189675));
#28435=CARTESIAN_POINT('Ctrl Pts',(-4.0305704817495,-72.6952744058323,26.9872349869563));
#28436=CARTESIAN_POINT('Ctrl Pts',(-4.01826668589923,-72.6895704554035,
26.9879839173813));
#28437=CARTESIAN_POINT('Ctrl Pts',(-4.00579082229074,-72.683782595724,26.9887104787675));
#28438=CARTESIAN_POINT('Ctrl Pts',(-3.9931476618675,-72.6779139798043,26.989411499818));
#28439=CARTESIAN_POINT('Ctrl Pts',(-3.97973438237103,-72.671687895269,26.990155221401));
#28440=CARTESIAN_POINT('Ctrl Pts',(-3.96613313239916,-72.6653710564959,
26.9908700643548));
#28441=CARTESIAN_POINT('Ctrl Pts',(-3.95240663901933,-72.658993520968,26.9915498852838));
#28442=CARTESIAN_POINT('Ctrl Pts',(-3.93749262433767,-72.6520642451608,
26.9922885196193));
#28443=CARTESIAN_POINT('Ctrl Pts',(-3.92243124975649,-72.6450635337329,
26.9929856248137));
#28444=CARTESIAN_POINT('Ctrl Pts',(-3.90736223915333,-72.6380574390472,
26.993633202471));
#28445=CARTESIAN_POINT('Ctrl Pts',(-3.88988346046555,-72.6299309613573,
26.994384337821));
#28446=CARTESIAN_POINT('Ctrl Pts',(-3.87239532264419,-72.6217976615962,
26.9950684921256));
#28447=CARTESIAN_POINT('Ctrl Pts',(-3.85518253073393,-72.6137916939521,
26.9956775890504));
#28448=CARTESIAN_POINT('Ctrl Pts',(-3.83312496894388,-72.6035323399252,
26.9964581244292));
#28449=CARTESIAN_POINT('Ctrl Pts',(-3.81152482888409,-72.5934845725453,
26.9971144521718));
#28450=CARTESIAN_POINT('Ctrl Pts',(-3.79103926538539,-72.5839576125555,
26.9976485299609));
#28451=CARTESIAN_POINT('Ctrl Pts',(-3.77639774349918,-72.5771484665337,
26.9980302481225));
#28452=CARTESIAN_POINT('Ctrl Pts',(-3.76232753448869,-72.5706062766685,
26.9983500673601));
#28453=CARTESIAN_POINT('Ctrl Pts',(-3.74904725004508,-72.5644337382693,
26.9986154588061));
#28454=CARTESIAN_POINT('Ctrl Pts',(-3.73712649404653,-72.5588930945835,
26.9988536816157));
#28455=CARTESIAN_POINT('Ctrl Pts',(-3.72584290510903,-72.55365061639,26.999048201826));
#28456=CARTESIAN_POINT('Ctrl Pts',(-3.71532050420447,-72.5487644340811,
26.9992071337773));
#28457=CARTESIAN_POINT('Ctrl Pts',(-3.70549567633381,-72.5442021768012,
26.9993555294789));
#28458=CARTESIAN_POINT('Ctrl Pts',(-3.69633489253103,-72.5399507407298,
26.9994729902421));
#28459=CARTESIAN_POINT('Ctrl Pts',(-3.68790009473844,-72.5360390514937,
26.9995669997594));
#28460=CARTESIAN_POINT('Ctrl Pts',(-3.67988122234412,-72.5323202502132,
26.9996563736059));
#28461=CARTESIAN_POINT('Ctrl Pts',(-3.67251881961981,-72.5289086594291,
26.9997246070627));
#28462=CARTESIAN_POINT('Ctrl Pts',(-3.66582431552888,-72.5258095023081,
26.9997779400933));
#28463=CARTESIAN_POINT('Ctrl Pts',(-3.65939305483032,-72.5228322112168,
26.9998291759458));
#28464=CARTESIAN_POINT('Ctrl Pts',(-3.6535784467587,-72.5201433779329,26.9998666884134));
#28465=CARTESIAN_POINT('Ctrl Pts',(-3.64834700663704,-72.5177272092178,
26.9998952450266));
#28466=CARTESIAN_POINT('Ctrl Pts',(-3.64336360571696,-72.51542559874,26.99992244768));
#28467=CARTESIAN_POINT('Ctrl Pts',(-3.63890946442555,-72.5133714448824,
26.9999415292289));
#28468=CARTESIAN_POINT('Ctrl Pts',(-3.63491308271419,-72.5115312156491,
26.999955676367));
#28469=CARTESIAN_POINT('Ctrl Pts',(-3.63100696390056,-72.509732550119,26.9999695039757));
#28470=CARTESIAN_POINT('Ctrl Pts',(-3.62753836258856,-72.5081383474962,
26.9999786149847));
#28471=CARTESIAN_POINT('Ctrl Pts',(-3.62439655959128,-72.5066967962248,
26.999985050899));
#28472=CARTESIAN_POINT('Ctrl Pts',(-3.62135346789029,-72.5053005365884,
26.9999912846053));
#28473=CARTESIAN_POINT('Ctrl Pts',(-3.61861704716632,-72.50404752535,26.9999950010979));
#28474=CARTESIAN_POINT('Ctrl Pts',(-3.61604301879889,-72.502870335936,26.9999972537214));
#28475=CARTESIAN_POINT('Ctrl Pts',(-3.61387203465112,-72.5018774721475,
26.9999991536266));
#28476=CARTESIAN_POINT('Ctrl Pts',(-3.61181592875733,-72.500938245988,27.));
#28477=CARTESIAN_POINT('Ctrl Pts',(-3.60976192857619,-72.5,27.));
#28478=CARTESIAN_POINT('',(-4.20488096428809,-72.2245134174903,27.));
#28479=CARTESIAN_POINT('Ctrl Pts',(-4.59286900030108,-72.9498135639877,
26.9309674201926));
#28480=CARTESIAN_POINT('Ctrl Pts',(-4.97872124829708,-73.1202082891348,
26.87740515349));
#28481=CARTESIAN_POINT('Ctrl Pts',(-5.39943703784252,-73.2960271674307,
26.7866344447428));
#28482=CARTESIAN_POINT('Ctrl Pts',(-6.23069890002426,-73.6032059786734,
26.5355629374701));
#28483=CARTESIAN_POINT('Ctrl Pts',(-6.64131282637154,-73.7333042369875,
26.3751846606466));
#28484=CARTESIAN_POINT('Ctrl Pts',(-7.41892283648103,-73.9255858170934,
26.0143833640028));
#28485=CARTESIAN_POINT('Ctrl Pts',(-7.86775357562107,-74.000000000199,25.7653963103419));
#28486=CARTESIAN_POINT('Ctrl Pts',(-8.27069753274498,-74.,25.4999999988754));
#28487=CARTESIAN_POINT('Ctrl Pts',(-4.73222742226463,-72.6487711068476,
26.9529185755998));
#28488=CARTESIAN_POINT('Ctrl Pts',(-5.11803926821329,-72.8218353520906,
26.9133538137028));
#28489=CARTESIAN_POINT('Ctrl Pts',(-5.5378193485972,-73.0038698341822,26.8373083736856));
#28490=CARTESIAN_POINT('Ctrl Pts',(-6.36525494892567,-73.3302744149464,
26.613175065831));
#28491=CARTESIAN_POINT('Ctrl Pts',(-6.77293386456173,-73.473510370804,26.4648562596415));
#28492=CARTESIAN_POINT('Ctrl Pts',(-7.5432142505923,-73.6962982209631,26.123992425085));
#28493=CARTESIAN_POINT('Ctrl Pts',(-7.98659795783503,-73.7922248094884,
25.8845123595807));
#28494=CARTESIAN_POINT('Ctrl Pts',(-8.38308611702755,-73.8157835060006,
25.6245617146941));
#28495=CARTESIAN_POINT('Ctrl Pts',(-4.87158584422818,-72.3477286497075,
26.974869731007));
#28496=CARTESIAN_POINT('Ctrl Pts',(-5.25729552724842,-72.5236704313501,
26.9492448421667));
#28497=CARTESIAN_POINT('Ctrl Pts',(-5.67620378478722,-72.7117042159167,
26.8879934646398));
#28498=CARTESIAN_POINT('Ctrl Pts',(-6.49978013406627,-73.0574406580189,
26.6907209397854));
#28499=CARTESIAN_POINT('Ctrl Pts',(-6.90453460491355,-73.2137788863189,
26.5544817167923));
#28500=CARTESIAN_POINT('Ctrl Pts',(-7.66749336352552,-73.4670504132414,
26.2335669039408));
#28501=CARTESIAN_POINT('Ctrl Pts',(-8.10533935929029,-73.5847724306284,
26.0033054888075));
#28502=CARTESIAN_POINT('Ctrl Pts',(-8.49547470131012,-73.6315670120013,
25.7491234305128));
#28503=CARTESIAN_POINT('Ctrl Pts',(-5.01094426619173,-72.0466861925674,
26.9968208864141));
#28504=CARTESIAN_POINT('Ctrl Pts',(-5.39661354716464,-72.2252974943058,
26.9851935023795));
#28505=CARTESIAN_POINT('Ctrl Pts',(-5.8145860955419,-72.4195468826682,26.9386673935825));
#28506=CARTESIAN_POINT('Ctrl Pts',(-6.63433618296768,-72.7845090942918,
26.7683330681463));
#28507=CARTESIAN_POINT('Ctrl Pts',(-7.03615564310373,-72.9539850201353,
26.6441533157873));
#28508=CARTESIAN_POINT('Ctrl Pts',(-7.7917847776368,-73.2377628171111,26.3431759650231));
#28509=CARTESIAN_POINT('Ctrl Pts',(-8.22418374150425,-73.3769972399179,
26.1224215380463));
#28510=CARTESIAN_POINT('Ctrl Pts',(-8.60786328559268,-73.4473505180019,
25.8736851463315));
#28511=CARTESIAN_POINT('',(-8.60786328559223,-73.4473505180018,25.8736851463318));
#28512=CARTESIAN_POINT('Ctrl Pts',(-5.01094426619173,-72.0466861925674,
26.9968208864141));
#28513=CARTESIAN_POINT('Ctrl Pts',(-5.39661354716464,-72.2252974943058,
26.9851935023795));
#28514=CARTESIAN_POINT('Ctrl Pts',(-5.8145860955419,-72.4195468826682,26.9386673935825));
#28515=CARTESIAN_POINT('Ctrl Pts',(-6.63433618296768,-72.7845090942918,
26.7683330681463));
#28516=CARTESIAN_POINT('Ctrl Pts',(-7.03615564310373,-72.9539850201353,
26.6441533157873));
#28517=CARTESIAN_POINT('Ctrl Pts',(-7.7917847776368,-73.2377628171111,26.3431759650231));
#28518=CARTESIAN_POINT('Ctrl Pts',(-8.22418374150425,-73.3769972399179,
26.1224215380463));
#28519=CARTESIAN_POINT('Ctrl Pts',(-8.60786328559268,-73.4473505180019,
25.8736851463315));
#28520=CARTESIAN_POINT('',(-8.27069753304877,-74.,25.4999999993376));
#28521=CARTESIAN_POINT('',(-8.60786328559223,-73.4473505180018,25.8736851463318));
#28522=CARTESIAN_POINT('Ctrl Pts',(-8.27069753274498,-74.,25.4999999988754));
#28523=CARTESIAN_POINT('Ctrl Pts',(-7.86775357562107,-74.000000000199,25.7653963103419));
#28524=CARTESIAN_POINT('Ctrl Pts',(-7.41892283648103,-73.9255858170934,
26.0143833640028));
#28525=CARTESIAN_POINT('Ctrl Pts',(-6.64131282637154,-73.7333042369875,
26.3751846606466));
#28526=CARTESIAN_POINT('Ctrl Pts',(-6.23069890002426,-73.6032059786734,
26.5355629374701));
#28527=CARTESIAN_POINT('Ctrl Pts',(-5.39943703784252,-73.2960271674307,
26.7866344447428));
#28528=CARTESIAN_POINT('Ctrl Pts',(-4.97872124829708,-73.1202082891348,
26.87740515349));
#28529=CARTESIAN_POINT('Ctrl Pts',(-4.59286900030108,-72.9498135639877,
26.9309674201926));
#28530=CARTESIAN_POINT('Origin',(-4.79999999999999,-73.75,20.));
#28531=CARTESIAN_POINT('',(-10.3,-73.5,24.3301270189222));
#28532=CARTESIAN_POINT('',(-9.90714285714286,-74.,24.0208322318563));
#28533=CARTESIAN_POINT('',(-10.3,-73.5,24.3301270189222));
#28534=CARTESIAN_POINT('',(-8.82083223185632,-74.,25.1071428571429));
#28535=CARTESIAN_POINT('Origin',(-4.79999999999999,-74.,20.));
#28536=CARTESIAN_POINT('',(-9.13012701892219,-73.5,25.5));
#28537=CARTESIAN_POINT('',(-8.82083223185632,-74.,25.1071428571429));
#28538=CARTESIAN_POINT('Origin',(-4.79999999999999,-73.5,20.));
#28539=CARTESIAN_POINT('Ctrl Pts',(-8.2706975327445,-74.,25.4999999988757));
#28540=CARTESIAN_POINT('Ctrl Pts',(-8.46780983228826,-74.,25.3701733162485));
#28541=CARTESIAN_POINT('Ctrl Pts',(-8.65244115216739,-74.,25.2397164505804));
#28542=CARTESIAN_POINT('Ctrl Pts',(-8.82083223185632,-74.,25.1071428571429));
#28543=CARTESIAN_POINT('Ctrl Pts',(-8.38308611702708,-73.8157835060006,
25.6245617146944));
#28544=CARTESIAN_POINT('Ctrl Pts',(-8.57705715860084,-73.8272553216869,
25.4974516009823));
#28545=CARTESIAN_POINT('Ctrl Pts',(-8.75893190880213,-73.8333333333333,
25.3679979349617));
#28546=CARTESIAN_POINT('Ctrl Pts',(-8.92393049421161,-73.8333333333333,
25.2380952380952));
#28547=CARTESIAN_POINT('Ctrl Pts',(-8.49547470130966,-73.6315670120012,
25.7491234305131));
#28548=CARTESIAN_POINT('Ctrl Pts',(-8.68630448491342,-73.6545106433737,
25.6247298857161));
#28549=CARTESIAN_POINT('Ctrl Pts',(-8.86542266543686,-73.6666666666667,
25.496279419343));
#28550=CARTESIAN_POINT('Ctrl Pts',(-9.0270287565669,-73.6666666666667,25.3690476190476));
#28551=CARTESIAN_POINT('Ctrl Pts',(-8.60786328559223,-73.4473505180018,
25.8736851463318));
#28552=CARTESIAN_POINT('Ctrl Pts',(-8.795551811226,-73.4817659650606,25.7520081704499));
#28553=CARTESIAN_POINT('Ctrl Pts',(-8.97191342207159,-73.5,25.6245609037243));
#28554=CARTESIAN_POINT('Ctrl Pts',(-9.13012701892219,-73.5,25.5));
#28555=CARTESIAN_POINT('Ctrl Pts',(-8.82083223185632,-74.,25.1071428571429));
#28556=CARTESIAN_POINT('Ctrl Pts',(-8.65244115216739,-74.,25.2397164505804));
#28557=CARTESIAN_POINT('Ctrl Pts',(-8.46780983228826,-74.,25.3701733162485));
#28558=CARTESIAN_POINT('Ctrl Pts',(-8.2706975327445,-74.,25.4999999988757));
#28559=CARTESIAN_POINT('Ctrl Pts',(-8.60786328559223,-73.4473505180018,
25.8736851463318));
#28560=CARTESIAN_POINT('Ctrl Pts',(-8.795551811226,-73.4817659650606,25.7520081704499));
#28561=CARTESIAN_POINT('Ctrl Pts',(-8.97191342207159,-73.5,25.6245609037243));
#28562=CARTESIAN_POINT('Ctrl Pts',(-9.13012701892219,-73.5,25.5));
#28563=CARTESIAN_POINT('Ctrl Pts',(-10.299999999979,-74.,23.4706975310694));
#28564=CARTESIAN_POINT('Ctrl Pts',(-10.6578919709938,-74.000000000005,22.9273199449621));
#28565=CARTESIAN_POINT('Ctrl Pts',(-11.3040157101811,-73.7466600445013,
21.7070019367622));
#28566=CARTESIAN_POINT('Ctrl Pts',(-11.645906962903,-73.2204120541234,20.4056287461521));
#28567=CARTESIAN_POINT('Ctrl Pts',(-11.7309675556501,-72.9498131330638,
19.7928680244678));
#28568=CARTESIAN_POINT('Ctrl Pts',(-10.4245617157746,-73.8157835059031,
23.5830861153787));
#28569=CARTESIAN_POINT('Ctrl Pts',(-10.7749649472824,-73.7841592615321,
23.0483680049966));
#28570=CARTESIAN_POINT('Ctrl Pts',(-11.3929741147526,-73.4750024331891,
21.8418287216067));
#28571=CARTESIAN_POINT('Ctrl Pts',(-11.6900564874004,-72.9237209037276,
20.5448942447467));
#28572=CARTESIAN_POINT('Ctrl Pts',(-11.7529186757946,-72.648770667648,19.9322264436722));
#28573=CARTESIAN_POINT('Ctrl Pts',(-10.5491234315702,-73.6315670118063,
23.6954746996879));
#28574=CARTESIAN_POINT('Ctrl Pts',(-10.892037923571,-73.5683185230592,23.1694160650311));
#28575=CARTESIAN_POINT('Ctrl Pts',(-11.4819325193241,-73.203344821877,21.9766555064513));
#28576=CARTESIAN_POINT('Ctrl Pts',(-11.7342060118978,-72.6270297533319,
20.6841597433414));
#28577=CARTESIAN_POINT('Ctrl Pts',(-11.7748697959391,-72.3477282022321,
20.0715848628766));
#28578=CARTESIAN_POINT('Ctrl Pts',(-10.6736851473658,-73.4473505177094,
23.8078632839972));
#28579=CARTESIAN_POINT('Ctrl Pts',(-11.0091108998596,-73.3524777845862,
23.2904641250657));
#28580=CARTESIAN_POINT('Ctrl Pts',(-11.5708909238955,-72.9316872105648,
22.1114822912959));
#28581=CARTESIAN_POINT('Ctrl Pts',(-11.7783555363952,-72.3303386029362,
20.823425241936));
#28582=CARTESIAN_POINT('Ctrl Pts',(-11.7968209160836,-72.0466857368163,
20.210943282081));
#28583=CARTESIAN_POINT('',(-10.2999999999876,-74.,23.4706975310751));
#28584=CARTESIAN_POINT('Ctrl Pts',(-11.7309675556501,-72.9498131330638,
19.7928680244678));
#28585=CARTESIAN_POINT('Ctrl Pts',(-11.645906962903,-73.2204120541234,20.4056287461521));
#28586=CARTESIAN_POINT('Ctrl Pts',(-11.3040157101811,-73.7466600445013,
21.7070019367622));
#28587=CARTESIAN_POINT('Ctrl Pts',(-10.6578919709938,-74.000000000005,22.9273199449621));
#28588=CARTESIAN_POINT('Ctrl Pts',(-10.299999999979,-74.,23.4706975310694));
#28589=CARTESIAN_POINT('',(-10.6736851473658,-73.4473505177094,23.8078632839972));
#28590=CARTESIAN_POINT('',(-10.2999999999876,-74.,23.4706975310751));
#28591=CARTESIAN_POINT('Ctrl Pts',(-10.6736851473658,-73.4473505177094,
23.8078632839972));
#28592=CARTESIAN_POINT('Ctrl Pts',(-11.0091108998596,-73.3524777845862,
23.2904641250657));
#28593=CARTESIAN_POINT('Ctrl Pts',(-11.5708909238955,-72.9316872105648,
22.1114822912959));
#28594=CARTESIAN_POINT('Ctrl Pts',(-11.7783555363952,-72.3303386029362,
20.823425241936));
#28595=CARTESIAN_POINT('Ctrl Pts',(-11.7968209160836,-72.0466857368163,
20.210943282081));
#28596=CARTESIAN_POINT('Ctrl Pts',(-9.90714285714286,-74.,24.0208322318563));
#28597=CARTESIAN_POINT('Ctrl Pts',(-10.0446625272125,-74.,23.8461587910824));
#28598=CARTESIAN_POINT('Ctrl Pts',(-10.1730966676381,-74.,23.6633713879345));
#28599=CARTESIAN_POINT('Ctrl Pts',(-10.299999999979,-74.,23.4706975310694));
#28600=CARTESIAN_POINT('Ctrl Pts',(-10.0380952380952,-73.8333333333333,
24.1239304942116));
#28601=CARTESIAN_POINT('Ctrl Pts',(-10.1728443653613,-73.8333333333333,
23.9527761154313));
#28602=CARTESIAN_POINT('Ctrl Pts',(-10.3003137824798,-73.8269970069562,
23.7726894470159));
#28603=CARTESIAN_POINT('Ctrl Pts',(-10.4245617157746,-73.8157835059031,
23.5830861153787));
#28604=CARTESIAN_POINT('Ctrl Pts',(-10.1690476190476,-73.6666666666667,
24.2270287565669));
#28605=CARTESIAN_POINT('Ctrl Pts',(-10.3010262035101,-73.6666666666667,
24.0593934397802));
#28606=CARTESIAN_POINT('Ctrl Pts',(-10.4275308973216,-73.6539940139125,
23.8820075060973));
#28607=CARTESIAN_POINT('Ctrl Pts',(-10.5491234315702,-73.6315670118063,
23.6954746996879));
#28608=CARTESIAN_POINT('Ctrl Pts',(-10.3,-73.5,24.3301270189222));
#28609=CARTESIAN_POINT('Ctrl Pts',(-10.4292080416589,-73.5,24.1660107641291));
#28610=CARTESIAN_POINT('Ctrl Pts',(-10.5547480121633,-73.4809910208688,
23.9913255651787));
#28611=CARTESIAN_POINT('Ctrl Pts',(-10.6736851473658,-73.4473505177094,
23.8078632839972));
#28612=CARTESIAN_POINT('Ctrl Pts',(-10.299999999979,-74.,23.4706975310694));
#28613=CARTESIAN_POINT('Ctrl Pts',(-10.1730966676381,-74.,23.6633713879345));
#28614=CARTESIAN_POINT('Ctrl Pts',(-10.0446625272125,-74.,23.8461587910824));
#28615=CARTESIAN_POINT('Ctrl Pts',(-9.90714285714286,-74.,24.0208322318563));
#28616=CARTESIAN_POINT('Ctrl Pts',(-10.3,-73.5,24.3301270189222));
#28617=CARTESIAN_POINT('Ctrl Pts',(-10.4292080416589,-73.5,24.1660107641291));
#28618=CARTESIAN_POINT('Ctrl Pts',(-10.5547480121633,-73.4809910208688,
23.9913255651787));
#28619=CARTESIAN_POINT('Ctrl Pts',(-10.6736851473658,-73.4473505177094,
23.8078632839972));
#28620=CARTESIAN_POINT('Origin',(-10.3,-72.5,10.));
#28621=CARTESIAN_POINT('',(-10.3,-74.,10.));
#28622=CARTESIAN_POINT('',(-11.8,-72.5,10.));
#28623=CARTESIAN_POINT('Origin',(-11.8,-32.,20.));
#28624=CARTESIAN_POINT('',(-11.8,-32.,20.));
#28625=CARTESIAN_POINT('Origin',(-4.79999999999999,-32.,20.));
#28626=CARTESIAN_POINT('',(-4.8,-32.,27.));
#28627=CARTESIAN_POINT('Origin',(28.2,-73.75,-3.99999999999999));
#28628=CARTESIAN_POINT('',(28.2,-74.,-11.5));
#28629=CARTESIAN_POINT('',(28.2,-73.5,-11.));
#28630=CARTESIAN_POINT('',(35.7,-74.,-4.));
#28631=CARTESIAN_POINT('Origin',(28.2,-74.,-3.99999999999999));
#28632=CARTESIAN_POINT('',(35.7,-74.,-4.));
#28633=CARTESIAN_POINT('Origin',(21.7,-73.75,-11.25));
#28634=CARTESIAN_POINT('',(2.2,-74.,-11.5));
#28635=CARTESIAN_POINT('',(2.2,-73.5,-11.));
#28636=CARTESIAN_POINT('',(21.7,-74.,-11.5));
#28637=CARTESIAN_POINT('Origin',(2.2,-73.75,-4.));
#28638=CARTESIAN_POINT('',(-5.3,-74.,-4.));
#28639=CARTESIAN_POINT('',(-4.8,-73.5,-4.));
#28640=CARTESIAN_POINT('Origin',(2.2,-74.,-4.));
#28641=CARTESIAN_POINT('Origin',(-5.05,-73.75,-2.));
#28642=CARTESIAN_POINT('',(-5.3,-74.,4.));
#28643=CARTESIAN_POINT('',(-4.8,-73.5,4.));
#28644=CARTESIAN_POINT('',(-5.3,-74.,-2.));
#28645=CARTESIAN_POINT('Origin',(2.2,-73.75,4.));
#28646=CARTESIAN_POINT('',(2.2,-73.5,11.));
#28647=CARTESIAN_POINT('',(2.2,-74.,11.5));
#28648=CARTESIAN_POINT('',(2.2,-73.5,11.));
#28649=CARTESIAN_POINT('Origin',(2.2,-74.,4.));
#28650=CARTESIAN_POINT('Origin',(2.2,-73.5,4.));
#28651=CARTESIAN_POINT('Origin',(8.7,-73.75,11.25));
#28652=CARTESIAN_POINT('',(28.2,-73.5,11.));
#28653=CARTESIAN_POINT('',(28.2,-74.,11.5));
#28654=CARTESIAN_POINT('',(28.2,-73.5,11.));
#28655=CARTESIAN_POINT('',(8.7,-74.,11.5));
#28656=CARTESIAN_POINT('',(8.7,-73.5,11.));
#28657=CARTESIAN_POINT('Origin',(28.2,-73.75,3.99999999999999));
#28658=CARTESIAN_POINT('',(35.2,-73.5,4.));
#28659=CARTESIAN_POINT('',(35.7,-74.,4.));
#28660=CARTESIAN_POINT('',(35.2,-73.5,4.));
#28661=CARTESIAN_POINT('Origin',(28.2,-74.,3.99999999999999));
#28662=CARTESIAN_POINT('Origin',(28.2,-73.5,3.99999999999999));
#28663=CARTESIAN_POINT('Origin',(35.45,-73.75,2.));
#28664=CARTESIAN_POINT('',(35.7,-74.,2.));
#28665=CARTESIAN_POINT('',(35.2,-73.5,2.));
#28666=CARTESIAN_POINT('Origin',(15.2,-74.,0.));
#28667=CARTESIAN_POINT('',(39.2208322318563,-74.,-25.1071428571429));
#28668=CARTESIAN_POINT('Ctrl Pts',(39.2208322318563,-74.,-25.1071428571429));
#28669=CARTESIAN_POINT('Ctrl Pts',(39.0524411521674,-74.,-25.2397164505804));
#28670=CARTESIAN_POINT('Ctrl Pts',(38.8678098322883,-74.,-25.3701733162485));
#28671=CARTESIAN_POINT('Ctrl Pts',(38.6706975327445,-74.,-25.4999999988757));
#28672=CARTESIAN_POINT('',(40.3071428571429,-74.,-24.0208322318563));
#28673=CARTESIAN_POINT('Origin',(35.2,-74.,-20.));
#28674=CARTESIAN_POINT('',(40.6999999999876,-74.,-23.4706975310751));
#28675=CARTESIAN_POINT('Ctrl Pts',(40.699999999979,-74.,-23.4706975310694));
#28676=CARTESIAN_POINT('Ctrl Pts',(40.5730966676381,-74.,-23.6633713879345));
#28677=CARTESIAN_POINT('Ctrl Pts',(40.4446625272125,-74.,-23.8461587910824));
#28678=CARTESIAN_POINT('Ctrl Pts',(40.3071428571429,-74.,-24.0208322318563));
#28679=CARTESIAN_POINT('',(40.6999999999876,-74.,23.4706975310751));
#28680=CARTESIAN_POINT('',(40.7,-74.,-10.));
#28681=CARTESIAN_POINT('',(40.3071428571429,-74.,24.0208322318563));
#28682=CARTESIAN_POINT('Ctrl Pts',(40.3071428571429,-74.,24.0208322318563));
#28683=CARTESIAN_POINT('Ctrl Pts',(40.4446625272125,-74.,23.8461587910824));
#28684=CARTESIAN_POINT('Ctrl Pts',(40.5730966676381,-74.,23.6633713879345));
#28685=CARTESIAN_POINT('Ctrl Pts',(40.699999999979,-74.,23.4706975310694));
#28686=CARTESIAN_POINT('',(39.2208322318563,-74.,25.1071428571429));
#28687=CARTESIAN_POINT('Origin',(35.2,-74.,20.));
#28688=CARTESIAN_POINT('',(38.6706975330488,-74.,25.4999999993376));
#28689=CARTESIAN_POINT('Ctrl Pts',(38.6706975327445,-74.,25.4999999988757));
#28690=CARTESIAN_POINT('Ctrl Pts',(38.8678098322883,-74.,25.3701733162485));
#28691=CARTESIAN_POINT('Ctrl Pts',(39.0524411521674,-74.,25.2397164505804));
#28692=CARTESIAN_POINT('Ctrl Pts',(39.2208322318563,-74.,25.1071428571429));
#28693=CARTESIAN_POINT('',(25.2,-74.,25.5));
#28694=CARTESIAN_POINT('Ctrl Pts',(42.1309675556502,-72.9498131330638,-19.7928680244677));
#28695=CARTESIAN_POINT('Ctrl Pts',(42.131923849979,-72.9467709227376,-19.7859790576246));
#28696=CARTESIAN_POINT('Ctrl Pts',(42.133797063601,-72.9403541455888,-19.7715233813563));
#28697=CARTESIAN_POINT('Ctrl Pts',(42.1456478927983,-72.9035142121456,-19.6878036355088));
#28698=CARTESIAN_POINT('Ctrl Pts',(42.1734428705064,-72.7907445730559,-19.4364940183831));
#28699=CARTESIAN_POINT('Ctrl Pts',(42.1924901636104,-72.6655767127841,-19.1664431126415));
#28700=CARTESIAN_POINT('Ctrl Pts',(42.2001344080601,-72.5485934007217,-18.915145489479));
#28701=CARTESIAN_POINT('Ctrl Pts',(42.1998426464822,-72.5097904998462,-18.8311910013897));
#28702=CARTESIAN_POINT('Ctrl Pts',(42.2,-72.5031610690666,-18.8166823681909));
#28703=CARTESIAN_POINT('Ctrl Pts',(42.2,-72.5,-18.8097619285762));
#28704=CARTESIAN_POINT('Ctrl Pts',(42.1529186757946,-72.648770667648,-19.9322264436722));
#28705=CARTESIAN_POINT('Ctrl Pts',(42.1533741068936,-72.646492978889,-19.9271259487491));
#28706=CARTESIAN_POINT('Ctrl Pts',(42.1541647577967,-72.6424665483818,-19.9181031879452));
#28707=CARTESIAN_POINT('Ctrl Pts',(42.1623825078698,-72.6172309744667,-19.8602288521345));
#28708=CARTESIAN_POINT('Ctrl Pts',(42.1851067535948,-72.5287881205757,-19.662281685792));
#28709=CARTESIAN_POINT('Ctrl Pts',(42.1974831260006,-72.4421778837754,-19.4764677420227));
#28710=CARTESIAN_POINT('Ctrl Pts',(42.2015588908678,-72.3497072427885,-19.2786154621961));
#28711=CARTESIAN_POINT('Ctrl Pts',(42.1999951134572,-72.3228008493618,-19.2206366736043));
#28712=CARTESIAN_POINT('Ctrl Pts',(42.2,-72.3186768516068,-19.2116122804521));
#28713=CARTESIAN_POINT('Ctrl Pts',(42.2,-72.3163422783269,-19.2065079523841));
#28714=CARTESIAN_POINT('Ctrl Pts',(42.1748697959391,-72.3477282022321,-20.0715848628766));
#28715=CARTESIAN_POINT('Ctrl Pts',(42.1750197265735,-72.3462456838324,-20.0683082748074));
#28716=CARTESIAN_POINT('Ctrl Pts',(42.1755923536803,-72.3423623098006,-20.0597599196363));
#28717=CARTESIAN_POINT('Ctrl Pts',(42.1789294016785,-72.3223172427598,-20.0158885701159));
#28718=CARTESIAN_POINT('Ctrl Pts',(42.1857191167759,-72.2729880555877,-19.9084435042539));
#28719=CARTESIAN_POINT('Ctrl Pts',(42.1947085871064,-72.2076838276853,-19.7662744561243));
#28720=CARTESIAN_POINT('Ctrl Pts',(42.1983926835278,-72.1582937197183,-19.658974397133));
#28721=CARTESIAN_POINT('Ctrl Pts',(42.1997583650979,-72.138122537015,-19.6151072161929));
#28722=CARTESIAN_POINT('Ctrl Pts',(42.2,-72.134192634147,-19.6065421927134));
#28723=CARTESIAN_POINT('Ctrl Pts',(42.2,-72.1326845566538,-19.6032539761921));
#28724=CARTESIAN_POINT('Ctrl Pts',(42.1968209160836,-72.0466857368163,-20.2109432820811));
#28725=CARTESIAN_POINT('Ctrl Pts',(42.1968652729023,-72.0460043569063,-20.2094720016796));
#28726=CARTESIAN_POINT('Ctrl Pts',(42.1969519717285,-72.0445740919435,-20.2063835241584));
#28727=CARTESIAN_POINT('Ctrl Pts',(42.1975052667492,-72.0362656373519,-20.1884440303172));
#28728=CARTESIAN_POINT('Ctrl Pts',(42.1987929410797,-72.0112736650882,-20.1344713791154));
#28729=CARTESIAN_POINT('Ctrl Pts',(42.1996557903764,-71.9844299252291,-20.0764806253147));
#28730=CARTESIAN_POINT('Ctrl Pts',(42.2000060026571,-71.9594531297301,-20.0225217576406));
#28731=CARTESIAN_POINT('Ctrl Pts',(42.199992764164,-71.9511381123642,-20.0045600356903));
#28732=CARTESIAN_POINT('Ctrl Pts',(42.2,-71.9497084166872,-20.0014721049746));
#28733=CARTESIAN_POINT('Ctrl Pts',(42.2,-71.9490268349807,-20.));
#28734=CARTESIAN_POINT('',(42.1309675556502,-72.9498131330638,-19.7928680244677));
#28735=CARTESIAN_POINT('Ctrl Pts',(42.2,-72.5,-18.8097619285762));
#28736=CARTESIAN_POINT('Ctrl Pts',(42.2,-72.501104434069,-18.8121798350255));
#28737=CARTESIAN_POINT('Ctrl Pts',(42.199998844824,-72.5022107400032,-18.8146017627203));
#28738=CARTESIAN_POINT('Ctrl Pts',(42.1999961395225,-72.5034031482093,-18.8172080904455));
#28739=CARTESIAN_POINT('Ctrl Pts',(42.1999933680139,-72.5046247382961,-18.8198782029923));
#28740=CARTESIAN_POINT('Ctrl Pts',(42.1999889720745,-72.5059366396841,-18.8227417275941));
#28741=CARTESIAN_POINT('Ctrl Pts',(42.1999817153247,-72.5074063278034,-18.8259430216939));
#28742=CARTESIAN_POINT('Ctrl Pts',(42.1999742566232,-72.5089169166043,-18.8292334061994));
#28743=CARTESIAN_POINT('Ctrl Pts',(42.1999637834255,-72.5105941315298,-18.83288047915));
#28744=CARTESIAN_POINT('Ctrl Pts',(42.1999480152244,-72.5124880592726,-18.8369912426304));
#28745=CARTESIAN_POINT('Ctrl Pts',(42.199931738317,-72.5144430880226,-18.8412346256315));
#28746=CARTESIAN_POINT('Ctrl Pts',(42.1999098218899,-72.5166289622411,-18.8459719331802));
#28747=CARTESIAN_POINT('Ctrl Pts',(42.1998786784034,-72.519077475485,-18.8512709182691));
#28748=CARTESIAN_POINT('Ctrl Pts',(42.1998456108804,-72.521677257239,-18.8568972732759));
#28749=CARTESIAN_POINT('Ctrl Pts',(42.1998021319534,-72.5245731226336,-18.8631568226207));
#28750=CARTESIAN_POINT('Ctrl Pts',(42.1997427762118,-72.5277777824962,-18.8700764316876));
#28751=CARTESIAN_POINT('Ctrl Pts',(42.1996802900758,-72.5311514546458,-18.8773609777533));
#28752=CARTESIAN_POINT('Ctrl Pts',(42.1996001669454,-72.5348672363335,-18.885376785242));
#28753=CARTESIAN_POINT('Ctrl Pts',(42.1994951564366,-72.5389136971141,-18.8940991505866));
#28754=CARTESIAN_POINT('Ctrl Pts',(42.1993826824823,-72.5432477533007,-18.9034414434035));
#28755=CARTESIAN_POINT('Ctrl Pts',(42.1992415706987,-72.5479610044146,-18.9135939447025));
#28756=CARTESIAN_POINT('Ctrl Pts',(42.1990629471554,-72.5530120784886,-18.9244681723167));
#28757=CARTESIAN_POINT('Ctrl Pts',(42.1988649429093,-72.5586111954687,-18.9365222565747));
#28758=CARTESIAN_POINT('Ctrl Pts',(42.1986206702861,-72.5646251589739,-18.949462607627));
#28759=CARTESIAN_POINT('Ctrl Pts',(42.1983202304374,-72.5709682116296,-18.9631064122639));
#28760=CARTESIAN_POINT('Ctrl Pts',(42.1979524431967,-72.5787331397672,-18.9798086482816));
#28761=CARTESIAN_POINT('Ctrl Pts',(42.1974999722516,-72.5869905301771,-18.9975635488969));
#28762=CARTESIAN_POINT('Ctrl Pts',(42.1969538016202,-72.5955474532101,-19.0159607182467));
#28763=CARTESIAN_POINT('Ctrl Pts',(42.1963926885024,-72.6043384820296,-19.0348612091509));
#28764=CARTESIAN_POINT('Ctrl Pts',(42.1957325786725,-72.6134430509651,-19.0544340658138));
#28765=CARTESIAN_POINT('Ctrl Pts',(42.1949775407195,-72.6226464542665,-19.0742232187686));
#28766=CARTESIAN_POINT('Ctrl Pts',(42.1943746852057,-72.6299948562963,-19.0900237489613));
#28767=CARTESIAN_POINT('Ctrl Pts',(42.1937117025218,-72.6374056335292,-19.1059608261784));
#28768=CARTESIAN_POINT('Ctrl Pts',(42.1929961401609,-72.6447844102958,-19.121834298351));
#28769=CARTESIAN_POINT('Ctrl Pts',(42.192357485478,-72.6513701260813,-19.13600171113));
#28770=CARTESIAN_POINT('Ctrl Pts',(42.1916771251311,-72.6579301278482,-19.1501179668197));
#28771=CARTESIAN_POINT('Ctrl Pts',(42.1909619574118,-72.6644154541118,-19.164079711081));
#28772=CARTESIAN_POINT('Ctrl Pts',(42.1902956522372,-72.6704576821534,-19.1770875443427));
#28773=CARTESIAN_POINT('Ctrl Pts',(42.1895992563686,-72.67643494612,-19.1899609298698));
#28774=CARTESIAN_POINT('Ctrl Pts',(42.1888777417672,-72.6823268221358,-19.2026576733762));
#28775=CARTESIAN_POINT('Ctrl Pts',(42.188192629382,-72.687921438271,-19.2147138344182));
#28776=CARTESIAN_POINT('Ctrl Pts',(42.1874849648869,-72.693438960502,-19.2266104811067));
#28777=CARTESIAN_POINT('Ctrl Pts',(42.1867569121392,-72.6988815833764,-19.2383542485828));
#28778=CARTESIAN_POINT('Ctrl Pts',(42.1860580430634,-72.7041060411239,-19.2496272723423));
#28779=CARTESIAN_POINT('Ctrl Pts',(42.1853404669399,-72.7092614026533,-19.2607592299263));
#28780=CARTESIAN_POINT('Ctrl Pts',(42.1846028726667,-72.7143695651666,-19.2717996399122));
#28781=CARTESIAN_POINT('Ctrl Pts',(42.183851133165,-72.7195756895659,-19.2830517775752));
#28782=CARTESIAN_POINT('Ctrl Pts',(42.1830787256542,-72.724732519747,-19.2942082079408));
#28783=CARTESIAN_POINT('Ctrl Pts',(42.1822792532141,-72.729887397417,-19.3053745694477));
#28784=CARTESIAN_POINT('Ctrl Pts',(42.1815108442835,-72.7348419822639,-19.3161070618675));
#28785=CARTESIAN_POINT('Ctrl Pts',(42.1807168472024,-72.7397983610905,-19.3268566425136));
#28786=CARTESIAN_POINT('Ctrl Pts',(42.1798905612537,-72.7447936410782,-19.3377066031676));
#28787=CARTESIAN_POINT('Ctrl Pts',(42.1790348821558,-72.749966616221,-19.3489425252583));
#28788=CARTESIAN_POINT('Ctrl Pts',(42.1781445235793,-72.7551812136774,-19.3602859041663));
#28789=CARTESIAN_POINT('Ctrl Pts',(42.1772145611532,-72.7604556398254,-19.3717788059764));
#28790=CARTESIAN_POINT('Ctrl Pts',(42.1762202119558,-72.7660952455344,-19.3840674290118));
#28791=CARTESIAN_POINT('Ctrl Pts',(42.175180506677,-72.7718032174315,-19.3965269512495));
#28792=CARTESIAN_POINT('Ctrl Pts',(42.1740933204494,-72.7775768048783,-19.409153596826));
#28793=CARTESIAN_POINT('Ctrl Pts',(42.1729402752533,-72.7837001415259,-19.4225451323847));
#28794=CARTESIAN_POINT('Ctrl Pts',(42.1717337402546,-72.7898971149343,-19.4361243256636));
#28795=CARTESIAN_POINT('Ctrl Pts',(42.1704767177069,-72.7961388570958,-19.4498295830908));
#28796=CARTESIAN_POINT('Ctrl Pts',(42.1691117732258,-72.8029164853346,-19.4647115082577));
#28797=CARTESIAN_POINT('Ctrl Pts',(42.1676871916453,-72.8097466432141,-19.4797415851259));
#28798=CARTESIAN_POINT('Ctrl Pts',(42.1662147821111,-72.8165662848741,-19.4947816596442));
#28799=CARTESIAN_POINT('Ctrl Pts',(42.1645116079787,-72.8244547404951,-19.5121789022399));
#28800=CARTESIAN_POINT('Ctrl Pts',(42.1627442453548,-72.832328637204,-19.5295886154484));
#28801=CARTESIAN_POINT('Ctrl Pts',(42.1609440847193,-72.8400623197647,-19.5467306475705));
#28802=CARTESIAN_POINT('Ctrl Pts',(42.1585963565592,-72.8501484109563,-19.5690868921973));
#28803=CARTESIAN_POINT('Ctrl Pts',(42.1561926064094,-72.8599933687502,-19.5909825486671));
#28804=CARTESIAN_POINT('Ctrl Pts',(42.153829461459,-72.8692964892791,-19.611733851028));
#28805=CARTESIAN_POINT('Ctrl Pts',(42.1521606565976,-72.8758661636286,-19.626387998356));
#28806=CARTESIAN_POINT('Ctrl Pts',(42.1505129132781,-72.8821649104918,-19.6404694774991));
#28807=CARTESIAN_POINT('Ctrl Pts',(42.1489236489795,-72.8880982600165,-19.6537587709998));
#28808=CARTESIAN_POINT('Ctrl Pts',(42.1474976601363,-72.8934220379641,-19.6656827689679));
#28809=CARTESIAN_POINT('Ctrl Pts',(42.146118990168,-72.8984513774561,-19.6769682936815));
#28810=CARTESIAN_POINT('Ctrl Pts',(42.1448124401236,-72.9031339887235,-19.6874909539755));
#28811=CARTESIAN_POINT('Ctrl Pts',(42.1435926877886,-72.9075055212581,-19.6973145650335));
#28812=CARTESIAN_POINT('Ctrl Pts',(42.1424359361706,-72.9115747003091,-19.7064728666792));
#28813=CARTESIAN_POINT('Ctrl Pts',(42.1413577511395,-72.915316545818,-19.7149037671802));
#28814=CARTESIAN_POINT('Ctrl Pts',(42.1403328121502,-72.9188736007235,-19.7229183086448));
#28815=CARTESIAN_POINT('Ctrl Pts',(42.1393789657513,-72.9221347341472,-19.7302752031998));
#28816=CARTESIAN_POINT('Ctrl Pts',(42.1385035999543,-72.9250969217939,-19.7369630176399));
#28817=CARTESIAN_POINT('Ctrl Pts',(42.1376626969175,-72.9279424894365,-19.7433875358139));
#28818=CARTESIAN_POINT('Ctrl Pts',(42.1368942766262,-72.9305120885607,-19.7491943710542));
#28819=CARTESIAN_POINT('Ctrl Pts',(42.1361981280593,-72.9328220615438,-19.7544171202231));
#28820=CARTESIAN_POINT('Ctrl Pts',(42.1355350110767,-72.9350224285159,-19.7593920549341));
#28821=CARTESIAN_POINT('Ctrl Pts',(42.1349374860318,-72.9369871912694,-19.7638369366521));
#28822=CARTESIAN_POINT('Ctrl Pts',(42.1343986079509,-72.9387489413189,-19.7678234681457));
#28823=CARTESIAN_POINT('Ctrl Pts',(42.13387191165,-72.940470865567,-19.7717198808326));
#28824=CARTESIAN_POINT('Ctrl Pts',(42.1334012661809,-72.9419987635743,-19.7751782288515));
#28825=CARTESIAN_POINT('Ctrl Pts',(42.1329732356419,-72.9433821218023,-19.7783095280656));
#28826=CARTESIAN_POINT('Ctrl Pts',(42.1325586563635,-72.9447220067026,-19.7813424232698));
#28827=CARTESIAN_POINT('Ctrl Pts',(42.1321840603972,-72.9459262548977,-19.784068416823));
#28828=CARTESIAN_POINT('Ctrl Pts',(42.1318304518762,-72.9470587848148,-19.7866321657247));
#28829=CARTESIAN_POINT('Ctrl Pts',(42.1315331756714,-72.9480108947768,-19.7887874914539));
#28830=CARTESIAN_POINT('Ctrl Pts',(42.1312506313311,-72.948912598852,-19.7908287998052));
#28831=CARTESIAN_POINT('Ctrl Pts',(42.1309675556502,-72.9498131330638,-19.7928680244677));
#28832=CARTESIAN_POINT('Ctrl Pts',(42.1968209160836,-72.0466857368163,-20.2109432820811));
#28833=CARTESIAN_POINT('Ctrl Pts',(42.1748697959391,-72.3477282022321,-20.0715848628766));
#28834=CARTESIAN_POINT('Ctrl Pts',(42.1529186757946,-72.648770667648,-19.9322264436722));
#28835=CARTESIAN_POINT('Ctrl Pts',(42.1309675556502,-72.9498131330638,-19.7928680244677));
#28836=CARTESIAN_POINT('Ctrl Pts',(35.4109442661894,-72.0466861925664,-26.9968208864142));
#28837=CARTESIAN_POINT('Ctrl Pts',(35.4094729764645,-72.0460048083184,-26.9968652437211));
#28838=CARTESIAN_POINT('Ctrl Pts',(35.4063844798888,-72.044574534468,-26.9969519434978));
#28839=CARTESIAN_POINT('Ctrl Pts',(35.3884448933592,-72.0362660370501,-26.9975052438987));
#28840=CARTESIAN_POINT('Ctrl Pts',(35.3344720145561,-72.0112739574878,-26.9987929295366));
#28841=CARTESIAN_POINT('Ctrl Pts',(35.2764810198642,-71.9844300964231,-26.9996557867445));
#28842=CARTESIAN_POINT('Ctrl Pts',(35.2225218784051,-71.9594531763374,-27.0000060027141));
#28843=CARTESIAN_POINT('Ctrl Pts',(35.2045600608895,-71.9511381208737,-26.9999927640876));
#28844=CARTESIAN_POINT('Ctrl Pts',(35.2014721131251,-71.9497084193948,-27.));
#28845=CARTESIAN_POINT('Ctrl Pts',(35.2,-71.9490268349807,-27.));
#28846=CARTESIAN_POINT('Ctrl Pts',(35.2715858442274,-72.3477286497072,-26.9748697310069));
#28847=CARTESIAN_POINT('Ctrl Pts',(35.2683092255771,-72.3462461176061,-26.9750196643681));
#28848=CARTESIAN_POINT('Ctrl Pts',(35.2597589197381,-72.342362724116,-26.9755113943378));
#28849=CARTESIAN_POINT('Ctrl Pts',(35.2159130361133,-72.3223176226921,-26.9782700800717));
#28850=CARTESIAN_POINT('Ctrl Pts',(35.1085728978907,-72.2729884298032,-26.9845159160213));
#28851=CARTESIAN_POINT('Ctrl Pts',(34.9663896521622,-72.2076842086041,-26.9930983031639));
#28852=CARTESIAN_POINT('Ctrl Pts',(34.8590309097738,-72.1582939925205,-26.9980896019632));
#28853=CARTESIAN_POINT('Ctrl Pts',(34.8151119751847,-72.1381226464778,-26.99978388301));
#28854=CARTESIAN_POINT('Ctrl Pts',(34.8065421980393,-72.1341926745702,-27.));
#28855=CARTESIAN_POINT('Ctrl Pts',(34.8032539761921,-72.1326845566538,-27.));
#28856=CARTESIAN_POINT('Ctrl Pts',(35.1322274222654,-72.6487711068479,-26.9529185755996));
#28857=CARTESIAN_POINT('Ctrl Pts',(35.1271268758826,-72.6464933955941,-26.9533740167507));
#28858=CARTESIAN_POINT('Ctrl Pts',(35.1181040099963,-72.6425801185888,-26.954490007591));
#28859=CARTESIAN_POINT('Ctrl Pts',(35.0602294418299,-72.6159498143769,-26.9622965659357));
#28860=CARTESIAN_POINT('Ctrl Pts',(34.8622824530211,-72.5231676294432,-26.9782300245881));
#28861=CARTESIAN_POINT('Ctrl Pts',(34.6764682420516,-72.438402280726,-26.9937530473512));
#28862=CARTESIAN_POINT('Ctrl Pts',(34.4786155584546,-72.3480981199775,-26.9979624748782));
#28863=CARTESIAN_POINT('Ctrl Pts',(34.4206366861374,-72.322674383005,-26.9994067438287));
#28864=CARTESIAN_POINT('Ctrl Pts',(34.4116122829534,-72.3186769297456,-27.));
#28865=CARTESIAN_POINT('Ctrl Pts',(34.4065079523841,-72.3163422783269,-27.));
#28866=CARTESIAN_POINT('Ctrl Pts',(34.9928690003034,-72.9498135639887,-26.9309674201923));
#28867=CARTESIAN_POINT('Ctrl Pts',(34.9859799608414,-72.9467713218047,-26.9319237255421));
#28868=CARTESIAN_POINT('Ctrl Pts',(34.9715241428247,-72.9403544842611,-26.9337969592289));
#28869=CARTESIAN_POINT('Ctrl Pts',(34.8878040852748,-72.9035143512801,-26.9456478606198));
#28870=CARTESIAN_POINT('Ctrl Pts',(34.6364946325283,-72.7907448177968,-26.9734427948335));
#28871=CARTESIAN_POINT('Ctrl Pts',(34.3664435092558,-72.6655780479714,-26.9924899951682));
#28872=CARTESIAN_POINT('Ctrl Pts',(34.1151455412382,-72.5485944343277,-27.0001343924598));
#28873=CARTESIAN_POINT('Ctrl Pts',(34.0311910031954,-72.5097908429465,-26.9998426436926));
#28874=CARTESIAN_POINT('Ctrl Pts',(34.0166823678675,-72.503161184921,-27.));
#28875=CARTESIAN_POINT('Ctrl Pts',(34.0097619285762,-72.5,-27.));
#28876=CARTESIAN_POINT('Ctrl Pts',(34.9928690003034,-72.9498135639887,-26.9309674201923));
#28877=CARTESIAN_POINT('Ctrl Pts',(35.1322274222654,-72.6487711068479,-26.9529185755996));
#28878=CARTESIAN_POINT('Ctrl Pts',(35.2715858442274,-72.3477286497072,-26.9748697310069));
#28879=CARTESIAN_POINT('Ctrl Pts',(35.4109442661894,-72.0466861925664,-26.9968208864142));
#28880=CARTESIAN_POINT('Ctrl Pts',(34.9928690003034,-72.9498135639887,-26.9309674201923));
#28881=CARTESIAN_POINT('Ctrl Pts',(35.3787212463313,-73.1202082882644,-26.8774051537635));
#28882=CARTESIAN_POINT('Ctrl Pts',(35.7977539931684,-73.2955896700455,-26.7874092748223));
#28883=CARTESIAN_POINT('Ctrl Pts',(36.7538439760921,-73.6459407607355,-26.4950027398036));
#28884=CARTESIAN_POINT('Ctrl Pts',(37.5431082034452,-73.8929551961393,-26.1757552250324));
#28885=CARTESIAN_POINT('Ctrl Pts',(38.3641779127485,-74.0000000001514,-25.7018870729982));
#28886=CARTESIAN_POINT('Ctrl Pts',(38.670697532745,-74.,-25.4999999988754));
#28887=CARTESIAN_POINT('Ctrl Pts',(35.1322274222654,-72.6487711068479,-26.9529185755996));
#28888=CARTESIAN_POINT('Ctrl Pts',(35.5179816685701,-72.8220656430667,-26.9134786970919));
#28889=CARTESIAN_POINT('Ctrl Pts',(35.9362199946512,-73.003097605608,-26.8379018493463));
#28890=CARTESIAN_POINT('Ctrl Pts',(36.8877441571632,-73.376153426664,-26.5765090318869));
#28891=CARTESIAN_POINT('Ctrl Pts',(37.6709975247959,-73.6498315266744,-26.2802660100171));
#28892=CARTESIAN_POINT('Ctrl Pts',(38.4815957329272,-73.7974150709988,-25.8221481156266));
#28893=CARTESIAN_POINT('Ctrl Pts',(38.7830861170276,-73.8157835060006,-25.6245617146941));
#28894=CARTESIAN_POINT('Ctrl Pts',(35.2715858442274,-72.3477286497072,-26.9748697310069));
#28895=CARTESIAN_POINT('Ctrl Pts',(35.6573531268961,-72.5234401404136,-26.9491199589918));
#28896=CARTESIAN_POINT('Ctrl Pts',(36.0744840326391,-72.7114040323017,-26.888810351696));
#28897=CARTESIAN_POINT('Ctrl Pts',(37.021572601592,-73.1065740407313,-26.6577720692435));
#28898=CARTESIAN_POINT('Ctrl Pts',(37.7990763569512,-73.4059683812817,-26.3844509574549));
#28899=CARTESIAN_POINT('Ctrl Pts',(38.5985802916715,-73.5964176820098,-25.9426379705939));
#28900=CARTESIAN_POINT('Ctrl Pts',(38.8954747013101,-73.6315670120013,-25.7491234305128));
#28901=CARTESIAN_POINT('Ctrl Pts',(35.4109442661894,-72.0466861925664,-26.9968208864142));
#28902=CARTESIAN_POINT('Ctrl Pts',(35.7966135491349,-72.2252974952159,-26.9851935023203));
#28903=CARTESIAN_POINT('Ctrl Pts',(36.2129500341219,-72.4189119678641,-26.93930292622));
#28904=CARTESIAN_POINT('Ctrl Pts',(37.155472782663,-72.8367867066598,-26.7392783613268));
#28905=CARTESIAN_POINT('Ctrl Pts',(37.926965678302,-73.1628447118167,-26.4889617424396));
#28906=CARTESIAN_POINT('Ctrl Pts',(38.7159981118503,-73.3938327528572,-26.0628990132224));
#28907=CARTESIAN_POINT('Ctrl Pts',(39.0078632855927,-73.4473505180019,-25.8736851463315));
#28908=CARTESIAN_POINT('',(39.0078632855922,-73.4473505180018,-25.8736851463318));
#28909=CARTESIAN_POINT('Origin',(35.2,-73.75,-20.));
#28910=CARTESIAN_POINT('',(40.7,-73.5,-24.3301270189222));
#28911=CARTESIAN_POINT('',(39.2208322318563,-74.,-25.1071428571429));
#28912=CARTESIAN_POINT('Ctrl Pts',(38.6706975327445,-74.,-25.4999999988757));
#28913=CARTESIAN_POINT('Ctrl Pts',(38.8678098322883,-74.,-25.3701733162485));
#28914=CARTESIAN_POINT('Ctrl Pts',(39.0524411521674,-74.,-25.2397164505804));
#28915=CARTESIAN_POINT('Ctrl Pts',(39.2208322318563,-74.,-25.1071428571429));
#28916=CARTESIAN_POINT('Ctrl Pts',(38.7830861170271,-73.8157835060006,-25.6245617146944));
#28917=CARTESIAN_POINT('Ctrl Pts',(38.9770571586009,-73.8272553216869,-25.4974516009823));
#28918=CARTESIAN_POINT('Ctrl Pts',(39.1589319088021,-73.8333333333333,-25.3679979349617));
#28919=CARTESIAN_POINT('Ctrl Pts',(39.3239304942116,-73.8333333333333,-25.2380952380952));
#28920=CARTESIAN_POINT('Ctrl Pts',(38.8954747013097,-73.6315670120012,-25.7491234305131));
#28921=CARTESIAN_POINT('Ctrl Pts',(39.0863044849134,-73.6545106433737,-25.6247298857161));
#28922=CARTESIAN_POINT('Ctrl Pts',(39.2654226654369,-73.6666666666667,-25.496279419343));
#28923=CARTESIAN_POINT('Ctrl Pts',(39.4270287565669,-73.6666666666667,-25.3690476190476));
#28924=CARTESIAN_POINT('Ctrl Pts',(39.0078632855922,-73.4473505180018,-25.8736851463318));
#28925=CARTESIAN_POINT('Ctrl Pts',(39.195551811226,-73.4817659650606,-25.7520081704499));
#28926=CARTESIAN_POINT('Ctrl Pts',(39.3719134220716,-73.5,-25.6245609037243));
#28927=CARTESIAN_POINT('Ctrl Pts',(39.5301270189222,-73.5,-25.5));
#28928=CARTESIAN_POINT('Ctrl Pts',(40.699999999979,-74.,-23.4706975310694));
#28929=CARTESIAN_POINT('Ctrl Pts',(41.0578919709938,-74.000000000005,-22.9273199449621));
#28930=CARTESIAN_POINT('Ctrl Pts',(41.7040084948481,-73.7466609117147,-21.7069991633697));
#28931=CARTESIAN_POINT('Ctrl Pts',(42.0459069628923,-73.2204120541575,-20.4056287462293));
#28932=CARTESIAN_POINT('Ctrl Pts',(42.1309675556502,-72.9498131330637,-19.7928680244677));
#28933=CARTESIAN_POINT('Ctrl Pts',(40.8245617157746,-73.8157835059031,-23.5830861153787));
#28934=CARTESIAN_POINT('Ctrl Pts',(41.1749649472824,-73.7841592615321,-23.0483680049966));
#28935=CARTESIAN_POINT('Ctrl Pts',(41.7929663852314,-73.4750040339006,-21.8418257930973));
#28936=CARTESIAN_POINT('Ctrl Pts',(42.090056487394,-72.9237209037385,-20.5448942447724));
#28937=CARTESIAN_POINT('Ctrl Pts',(42.1529186757946,-72.648770667648,-19.9322264436722));
#28938=CARTESIAN_POINT('Ctrl Pts',(40.9491234315702,-73.6315670118063,-23.695474699688));
#28939=CARTESIAN_POINT('Ctrl Pts',(41.292037923571,-73.5683185230592,-23.1694160650312));
#28940=CARTESIAN_POINT('Ctrl Pts',(41.8819242756147,-73.2033471560866,-21.9766524228248));
#28941=CARTESIAN_POINT('Ctrl Pts',(42.1342060118958,-72.6270297533195,-20.6841597433155));
#28942=CARTESIAN_POINT('Ctrl Pts',(42.1748697959391,-72.3477282022321,-20.0715848628766));
#28943=CARTESIAN_POINT('Ctrl Pts',(41.0736851473658,-73.4473505177094,-23.8078632839972));
#28944=CARTESIAN_POINT('Ctrl Pts',(41.4091108998595,-73.3524777845863,-23.2904641250657));
#28945=CARTESIAN_POINT('Ctrl Pts',(41.9708821659981,-72.9316902782726,-22.1114790525524));
#28946=CARTESIAN_POINT('Ctrl Pts',(42.1783555363975,-72.3303386029005,-20.8234252418586));
#28947=CARTESIAN_POINT('Ctrl Pts',(42.1968209160836,-72.0466857368163,-20.2109432820811));
#28948=CARTESIAN_POINT('Ctrl Pts',(42.1309675556502,-72.9498131330637,-19.7928680244677));
#28949=CARTESIAN_POINT('Ctrl Pts',(42.0459069628923,-73.2204120541575,-20.4056287462293));
#28950=CARTESIAN_POINT('Ctrl Pts',(41.7040084948481,-73.7466609117147,-21.7069991633697));
#28951=CARTESIAN_POINT('Ctrl Pts',(41.0578919709938,-74.000000000005,-22.9273199449621));
#28952=CARTESIAN_POINT('Ctrl Pts',(40.699999999979,-74.,-23.4706975310694));
#28953=CARTESIAN_POINT('',(40.6999999999876,-74.,-23.4706975310751));
#28954=CARTESIAN_POINT('Ctrl Pts',(40.3071428571429,-74.,-24.0208322318563));
#28955=CARTESIAN_POINT('Ctrl Pts',(40.4446625272125,-74.,-23.8461587910824));
#28956=CARTESIAN_POINT('Ctrl Pts',(40.5730966676381,-74.,-23.6633713879345));
#28957=CARTESIAN_POINT('Ctrl Pts',(40.699999999979,-74.,-23.4706975310694));
#28958=CARTESIAN_POINT('Ctrl Pts',(40.4380952380952,-73.8333333333333,-24.1239304942116));
#28959=CARTESIAN_POINT('Ctrl Pts',(40.5728443653613,-73.8333333333333,-23.9527761154313));
#28960=CARTESIAN_POINT('Ctrl Pts',(40.7003137824798,-73.8269970069562,-23.7726894470159));
#28961=CARTESIAN_POINT('Ctrl Pts',(40.8245617157746,-73.8157835059031,-23.5830861153787));
#28962=CARTESIAN_POINT('Ctrl Pts',(40.5690476190476,-73.6666666666667,-24.2270287565669));
#28963=CARTESIAN_POINT('Ctrl Pts',(40.7010262035101,-73.6666666666667,-24.0593934397802));
#28964=CARTESIAN_POINT('Ctrl Pts',(40.8275308973216,-73.6539940139125,-23.8820075060973));
#28965=CARTESIAN_POINT('Ctrl Pts',(40.9491234315702,-73.6315670118063,-23.695474699688));
#28966=CARTESIAN_POINT('Ctrl Pts',(40.7,-73.5,-24.3301270189222));
#28967=CARTESIAN_POINT('Ctrl Pts',(40.8292080416589,-73.5,-24.1660107641291));
#28968=CARTESIAN_POINT('Ctrl Pts',(40.9547480121633,-73.4809910208687,-23.9913255651788));
#28969=CARTESIAN_POINT('Ctrl Pts',(41.0736851473658,-73.4473505177094,-23.8078632839972));
#28970=CARTESIAN_POINT('Origin',(40.7,-72.5,-10.));
#28971=CARTESIAN_POINT('',(42.1309672031646,-72.9498142544064,19.7928705636776));
#28972=CARTESIAN_POINT('Ctrl Pts',(42.1309672031646,-72.9498142544064,19.7928705636776));
#28973=CARTESIAN_POINT('Ctrl Pts',(42.1313015191887,-72.9487507148203,19.7904622190261));
#28974=CARTESIAN_POINT('Ctrl Pts',(42.131635265947,-72.9476850562422,19.7880498434514));
#28975=CARTESIAN_POINT('Ctrl Pts',(42.1319930273681,-72.9465377582794,19.7854527089951));
#28976=CARTESIAN_POINT('Ctrl Pts',(42.1323595522132,-72.9453623570669,19.7827919573092));
#28977=CARTESIAN_POINT('Ctrl Pts',(42.1327512677083,-72.9441013224905,19.7799374088966));
#28978=CARTESIAN_POINT('Ctrl Pts',(42.1331869934536,-72.9426906841072,19.7767444396953));
#28979=CARTESIAN_POINT('Ctrl Pts',(42.1336348579266,-72.9412407472539,19.7734625187076));
#28980=CARTESIAN_POINT('Ctrl Pts',(42.1341292064887,-72.9396328187942,19.7698232013363));
#28981=CARTESIAN_POINT('Ctrl Pts',(42.1346827212214,-72.9378190144668,19.7657193064195));
#28982=CARTESIAN_POINT('Ctrl Pts',(42.1352541149661,-72.935946622667,19.7614828520934));
#28983=CARTESIAN_POINT('Ctrl Pts',(42.1358885383903,-72.9338549128763,19.7567514907766));
#28984=CARTESIAN_POINT('Ctrl Pts',(42.1365920268532,-72.9315128600421,19.7514573859948));
#28985=CARTESIAN_POINT('Ctrl Pts',(42.1373390290756,-72.9290259412592,19.7458358182707));
#28986=CARTESIAN_POINT('Ctrl Pts',(42.1381638928087,-72.9262567586801,19.7395797654784));
#28987=CARTESIAN_POINT('Ctrl Pts',(42.1390652414578,-72.9231917187612,19.7326623902347));
#28988=CARTESIAN_POINT('Ctrl Pts',(42.140014214902,-72.9199647305237,19.7253795198202));
#28989=CARTESIAN_POINT('Ctrl Pts',(42.141047895993,-72.9164098916718,19.7173638532995));
#28990=CARTESIAN_POINT('Ctrl Pts',(42.1421560896575,-72.9125358324603,19.7086402766379));
#28991=CARTESIAN_POINT('Ctrl Pts',(42.1433432444181,-72.9083857384985,19.6992951270539));
#28992=CARTESIAN_POINT('Ctrl Pts',(42.144615779129,-72.9038694395542,19.6891379478677));
#28993=CARTESIAN_POINT('Ctrl Pts',(42.1459531129161,-72.8990233016358,19.6782576409165));
#28994=CARTESIAN_POINT('Ctrl Pts',(42.1474361260665,-72.8936492608903,19.6661921128894));
#28995=CARTESIAN_POINT('Ctrl Pts',(42.1489985826526,-72.8878698046632,19.653237905392));
#28996=CARTESIAN_POINT('Ctrl Pts',(42.1506057775466,-72.8817628559047,19.6395787815669));
#28997=CARTESIAN_POINT('Ctrl Pts',(42.1525799655489,-72.8742614228087,19.6228006804931));
#28998=CARTESIAN_POINT('Ctrl Pts',(42.1546209561383,-72.8662663804073,19.6049605042071));
#28999=CARTESIAN_POINT('Ctrl Pts',(42.1566625052706,-72.8579585810379,19.5864748262644));
#29000=CARTESIAN_POINT('Ctrl Pts',(42.1587486638376,-72.849469249798,19.567585221897));
#29001=CARTESIAN_POINT('Ctrl Pts',(42.1608345516525,-72.840655794778,19.5480271658165));
#29002=CARTESIAN_POINT('Ctrl Pts',(42.1628608842072,-72.831719811673,19.5282555859895));
#29003=CARTESIAN_POINT('Ctrl Pts',(42.1644778474499,-72.8245891182514,19.5124783544806));
#29004=CARTESIAN_POINT('Ctrl Pts',(42.1660570689819,-72.8173810964839,19.4965664787151));
#29005=CARTESIAN_POINT('Ctrl Pts',(42.1675779259144,-72.8101854789778,19.4807189369477));
#29006=CARTESIAN_POINT('Ctrl Pts',(42.1689362597088,-72.8037588058168,19.4665649089913));
#29007=CARTESIAN_POINT('Ctrl Pts',(42.1702481373004,-72.797342287202,19.4524626884228));
#29008=CARTESIAN_POINT('Ctrl Pts',(42.1715056420027,-72.7909830674702,19.438514996399));
#29009=CARTESIAN_POINT('Ctrl Pts',(42.1726775405847,-72.7850567591446,19.4255168100099));
#29010=CARTESIAN_POINT('Ctrl Pts',(42.1738022893872,-72.7791803848424,19.4126531571166));
#29011=CARTESIAN_POINT('Ctrl Pts',(42.1748785703465,-72.7733737418493,19.3999657009192));
#29012=CARTESIAN_POINT('Ctrl Pts',(42.1759006966771,-72.767859268473,19.3879166323786));
#29013=CARTESIAN_POINT('Ctrl Pts',(42.1768791687987,-72.7624078121534,19.3760267222246));
#29014=CARTESIAN_POINT('Ctrl Pts',(42.1778167095488,-72.7570170674844,19.3642888110875));
#29015=CARTESIAN_POINT('Ctrl Pts',(42.1787167504197,-72.7518419425355,19.3530203944763));
#29016=CARTESIAN_POINT('Ctrl Pts',(42.1795791195132,-72.7467228693616,19.3418922583279));
#29017=CARTESIAN_POINT('Ctrl Pts',(42.1804090975907,-72.7416379601195,19.33085433272));
#29018=CARTESIAN_POINT('Ctrl Pts',(42.1812615514281,-72.7364153518196,19.3195175007041));
#29019=CARTESIAN_POINT('Ctrl Pts',(42.1820798756141,-72.7312290975577,19.3082765013242));
#29020=CARTESIAN_POINT('Ctrl Pts',(42.1828722837951,-72.726030506685,19.2970223926875));
#29021=CARTESIAN_POINT('Ctrl Pts',(42.1836281590859,-72.7210715897002,19.2862871392632));
#29022=CARTESIAN_POINT('Ctrl Pts',(42.1843609603366,-72.7160979024093,19.2755321772426));
#29023=CARTESIAN_POINT('Ctrl Pts',(42.1850752052954,-72.7110725813951,19.2646751321278));
#29024=CARTESIAN_POINT('Ctrl Pts',(42.1858149431324,-72.7058678962916,19.2534305766423));
#29025=CARTESIAN_POINT('Ctrl Pts',(42.1865346966888,-72.7006079027222,19.242076712873));
#29026=CARTESIAN_POINT('Ctrl Pts',(42.1872349687888,-72.6952745441982,19.2305723771825));
#29027=CARTESIAN_POINT('Ctrl Pts',(42.1879839033092,-72.6895705666895,19.2182685967903));
#29028=CARTESIAN_POINT('Ctrl Pts',(42.188710468047,-72.6837826832338,19.2057927504724));
#29029=CARTESIAN_POINT('Ctrl Pts',(42.1894114918279,-72.6779140466942,19.1931496070932));
#29030=CARTESIAN_POINT('Ctrl Pts',(42.1901552158863,-72.6716879438093,19.1797363532756));
#29031=CARTESIAN_POINT('Ctrl Pts',(42.1908700606504,-72.6653710903413,19.1661351289144));
#29032=CARTESIAN_POINT('Ctrl Pts',(42.1915498829022,-72.6589935433102,19.1524086586535));
#29033=CARTESIAN_POINT('Ctrl Pts',(42.1922885178562,-72.6520642626857,19.137494685623));
#29034=CARTESIAN_POINT('Ctrl Pts',(42.1929856231885,-72.6450635503653,19.1224333500704));
#29035=CARTESIAN_POINT('Ctrl Pts',(42.1936332007538,-72.6380574576258,19.1073643725427));
#29036=CARTESIAN_POINT('Ctrl Pts',(42.1943843319655,-72.629931025811,19.0898857260347));
#29037=CARTESIAN_POINT('Ctrl Pts',(42.1950684825543,-72.6217977758197,19.0723977124727));
#29038=CARTESIAN_POINT('Ctrl Pts',(42.1956775765982,-72.6137918576236,19.0551850276049));
#29039=CARTESIAN_POINT('Ctrl Pts',(42.1964581307011,-72.6035322723288,19.0331269695248));
#29040=CARTESIAN_POINT('Ctrl Pts',(42.1971144713312,-72.5934842851803,19.0115263308462));
#29041=CARTESIAN_POINT('Ctrl Pts',(42.1976485567532,-72.5839571346295,18.9910403059571));
#29042=CARTESIAN_POINT('Ctrl Pts',(42.1980302734834,-72.5771479752563,18.9763987184592));
#29043=CARTESIAN_POINT('Ctrl Pts',(42.1983500908979,-72.5706057773694,18.9623284423976));
#29044=CARTESIAN_POINT('Ctrl Pts',(42.198615480378,-72.5644332365437,18.9490480914424));
#29045=CARTESIAN_POINT('Ctrl Pts',(42.1988537012205,-72.558892595386,18.9371272858667));
#29046=CARTESIAN_POINT('Ctrl Pts',(42.1990482194242,-72.5536501237203,18.9258436467134));
#29047=CARTESIAN_POINT('Ctrl Pts',(42.1992071494618,-72.5487639518768,18.9153211961306));
#29048=CARTESIAN_POINT('Ctrl Pts',(42.1993555433282,-72.5442017058562,18.9054963250792));
#29049=CARTESIAN_POINT('Ctrl Pts',(42.1994730023575,-72.5399502842729,18.8963354981348));
#29050=CARTESIAN_POINT('Ctrl Pts',(42.1995670103066,-72.5360386126285,18.8879006581744));
#29051=CARTESIAN_POINT('Ctrl Pts',(42.1996563826467,-72.5323198287168,18.8798817470811));
#29052=CARTESIAN_POINT('Ctrl Pts',(42.1997246147537,-72.5289082579991,18.8725193063125));
#29053=CARTESIAN_POINT('Ctrl Pts',(42.1997779466118,-72.5258091235177,18.8658247656506));
#29054=CARTESIAN_POINT('Ctrl Pts',(42.1998291813324,-72.5228318544961,18.859393470511));
#29055=CARTESIAN_POINT('Ctrl Pts',(42.1998666928339,-72.5201430455938,18.8535788292267));
#29056=CARTESIAN_POINT('Ctrl Pts',(42.1998952486401,-72.5177269034724,18.8483473578671));
#29057=CARTESIAN_POINT('Ctrl Pts',(42.1999224505203,-72.5154253187169,18.8433639280339));
#29058=CARTESIAN_POINT('Ctrl Pts',(42.1999415314425,-72.5133711925042,18.8389097594422));
#29059=CARTESIAN_POINT('Ctrl Pts',(42.1999556780803,-72.5115309927879,18.8349133527288));
#29060=CARTESIAN_POINT('Ctrl Pts',(42.1999695051995,-72.5097323561677,18.8310072096074));
#29061=CARTESIAN_POINT('Ctrl Pts',(42.1999786158394,-72.5081381842292,18.8275385861549));
#29062=CARTESIAN_POINT('Ctrl Pts',(42.199985051483,-72.5066966654099,18.824396763848));
#29063=CARTESIAN_POINT('Ctrl Pts',(42.1999912849262,-72.5053004374158,18.8213536539011));
#29064=CARTESIAN_POINT('Ctrl Pts',(42.1999950012483,-72.5040474594342,18.8186172174944));
#29065=CARTESIAN_POINT('Ctrl Pts',(42.1999972537806,-72.5028703049579,18.8160431766832));
#29066=CARTESIAN_POINT('Ctrl Pts',(42.1999991536502,-72.5018774490895,18.8138721349243));
#29067=CARTESIAN_POINT('Ctrl Pts',(42.2,-72.5009382344174,18.8118159788019));
#29068=CARTESIAN_POINT('Ctrl Pts',(42.2,-72.5,18.8097619285762));
#29069=CARTESIAN_POINT('Ctrl Pts',(40.699999999979,-74.,23.4706975310694));
#29070=CARTESIAN_POINT('Ctrl Pts',(41.0578917243185,-74.000000000005,22.9273203194824));
#29071=CARTESIAN_POINT('Ctrl Pts',(41.704007781412,-73.7466614991037,21.7070010142552));
#29072=CARTESIAN_POINT('Ctrl Pts',(42.0459074091364,-73.2204098933174,20.4056240222309));
#29073=CARTESIAN_POINT('Ctrl Pts',(42.1309672031646,-72.9498142544064,19.7928705636776));
#29074=CARTESIAN_POINT('Ctrl Pts',(34.9928678625178,-72.9498130615485,26.9309675781304));
#29075=CARTESIAN_POINT('Ctrl Pts',(34.9859788311223,-72.9467708226893,26.9319238812613));
#29076=CARTESIAN_POINT('Ctrl Pts',(34.9715230299339,-72.9403539923989,26.9337971106498));
#29077=CARTESIAN_POINT('Ctrl Pts',(34.8878030652082,-72.9035139065405,26.945647981921));
#29078=CARTESIAN_POINT('Ctrl Pts',(34.6364938840975,-72.7907445312107,26.9734428466108));
#29079=CARTESIAN_POINT('Ctrl Pts',(34.3664430831556,-72.6655778826375,26.9924900108967));
#29080=CARTESIAN_POINT('Ctrl Pts',(34.115145417116,-72.548594380104,27.0001343922656));
#29081=CARTESIAN_POINT('Ctrl Pts',(34.0311909778797,-72.5097908317003,26.9998426440259));
#29082=CARTESIAN_POINT('Ctrl Pts',(34.0166823597247,-72.5031611812015,27.));
#29083=CARTESIAN_POINT('Ctrl Pts',(34.0097619285762,-72.5,27.));
#29084=CARTESIAN_POINT('Ctrl Pts',(35.1322262809334,-72.648770594606,26.9529186924328));
#29085=CARTESIAN_POINT('Ctrl Pts',(35.127125742256,-72.6464928862312,26.9533741257474));
#29086=CARTESIAN_POINT('Ctrl Pts',(35.1181028925982,-72.6424664124947,26.9541647811871));
#29087=CARTESIAN_POINT('Ctrl Pts',(35.0602284162512,-72.6172306769364,26.9623825500304));
#29088=CARTESIAN_POINT('Ctrl Pts',(34.8622816998021,-72.5287879873221,26.985106682172));
#29089=CARTESIAN_POINT('Ctrl Pts',(34.6764678135481,-72.4421788390646,26.9974829453611));
#29090=CARTESIAN_POINT('Ctrl Pts',(34.4786154337669,-72.349707994528,27.0015588663316));
#29091=CARTESIAN_POINT('Ctrl Pts',(34.4206366608306,-72.3228010801069,26.9999951100012));
#29092=CARTESIAN_POINT('Ctrl Pts',(34.4116122748509,-72.3186769260278,27.));
#29093=CARTESIAN_POINT('Ctrl Pts',(34.4065079523841,-72.3163422783269,27.));
#29094=CARTESIAN_POINT('Ctrl Pts',(35.271584699349,-72.3477281276635,26.9748698067351));
#29095=CARTESIAN_POINT('Ctrl Pts',(35.2683080889331,-72.346245599186,26.9750197376988));
#29096=CARTESIAN_POINT('Ctrl Pts',(35.259759695035,-72.3423622132382,26.9755923652128));
#29097=CARTESIAN_POINT('Ctrl Pts',(35.2158882710644,-72.3223171563717,26.978929412466));
#29098=CARTESIAN_POINT('Ctrl Pts',(35.1084432567777,-72.2729880991628,26.9857191223274));
#29099=CARTESIAN_POINT('Ctrl Pts',(34.9662743319328,-72.2076840197809,26.9947085888439));
#29100=CARTESIAN_POINT('Ctrl Pts',(34.8589743510709,-72.1582939366101,26.9983926839512));
#29101=CARTESIAN_POINT('Ctrl Pts',(34.8151072057806,-72.1381226350592,26.9997583651705));
#29102=CARTESIAN_POINT('Ctrl Pts',(34.8065421899769,-72.1341926708542,27.));
#29103=CARTESIAN_POINT('Ctrl Pts',(34.8032539761921,-72.1326845566538,27.));
#29104=CARTESIAN_POINT('Ctrl Pts',(35.4109431177646,-72.046685660721,26.9968209210375));
#29105=CARTESIAN_POINT('Ctrl Pts',(35.4094718360417,-72.0460042802042,26.9968652778614));
#29106=CARTESIAN_POINT('Ctrl Pts',(35.4063833562612,-72.0445740141917,26.996951976694));
#29107=CARTESIAN_POINT('Ctrl Pts',(35.3884438670994,-72.0362655625548,26.9975052710777));
#29108=CARTESIAN_POINT('Ctrl Pts',(35.3344712811044,-72.0112736209447,26.9987929427077));
#29109=CARTESIAN_POINT('Ctrl Pts',(35.2764806026585,-71.9844299049754,26.9996557904983));
#29110=CARTESIAN_POINT('Ctrl Pts',(35.2225217556451,-71.9594531196762,27.0000060026486));
#29111=CARTESIAN_POINT('Ctrl Pts',(35.2045600360351,-71.9511381093811,26.9999927641665));
#29112=CARTESIAN_POINT('Ctrl Pts',(35.2014721051031,-71.9497084156806,27.));
#29113=CARTESIAN_POINT('Ctrl Pts',(35.2,-71.9490268349807,27.));
#29114=CARTESIAN_POINT('',(34.0097619285762,-72.5,27.));
#29115=CARTESIAN_POINT('',(34.9928678625178,-72.9498130615485,26.9309675781304));
#29116=CARTESIAN_POINT('Ctrl Pts',(34.0097619285762,-72.5,27.));
#29117=CARTESIAN_POINT('Ctrl Pts',(34.0121798317656,-72.5011044731095,27.));
#29118=CARTESIAN_POINT('Ctrl Pts',(34.0146017561988,-72.5022108180881,26.9999988447398));
#29119=CARTESIAN_POINT('Ctrl Pts',(34.0172080806341,-72.5034032651581,26.9999961392571));
#29120=CARTESIAN_POINT('Ctrl Pts',(34.0198781898187,-72.5046248950636,26.999993367563));
#29121=CARTESIAN_POINT('Ctrl Pts',(34.0227417110302,-72.5059368360811,26.9999889713356));
#29122=CARTESIAN_POINT('Ctrl Pts',(34.0259430017054,-72.5074065633977,26.9999817141614));
#29123=CARTESIAN_POINT('Ctrl Pts',(34.0292333827049,-72.5089171924931,26.9999742550237));
#29124=CARTESIAN_POINT('Ctrl Pts',(34.0328804521166,-72.5105944472574,26.9999637812448));
#29125=CARTESIAN_POINT('Ctrl Pts',(34.0369912120385,-72.5124884140809,26.9999480122703));
#29126=CARTESIAN_POINT('Ctrl Pts',(34.0412345913922,-72.5144434831844,26.9999317345645));
#29127=CARTESIAN_POINT('Ctrl Pts',(34.0459718952787,-72.5166293969508,26.9999098171331));
#29128=CARTESIAN_POINT('Ctrl Pts',(34.0512708767212,-72.5190779485735,26.999878672386));
#29129=CARTESIAN_POINT('Ctrl Pts',(34.0568972279557,-72.5216777711233,26.9998456035239));
#29130=CARTESIAN_POINT('Ctrl Pts',(34.0631567735687,-72.5245736760052,26.9998021229674));
#29131=CARTESIAN_POINT('Ctrl Pts',(34.070076378992,-72.5277783735895,26.9997427652637));
#29132=CARTESIAN_POINT('Ctrl Pts',(34.0773609213403,-72.531152085505,26.9996802770609));
#29133=CARTESIAN_POINT('Ctrl Pts',(34.0853767252336,-72.5348679050113,26.9996001514933));
#29134=CARTESIAN_POINT('Ctrl Pts',(34.0940990871599,-72.5389144011236,26.9994951381666));
#29135=CARTESIAN_POINT('Ctrl Pts',(34.1034413765545,-72.5432484952639,26.9993826611911));
#29136=CARTESIAN_POINT('Ctrl Pts',(34.1135938746767,-72.5479617814953,26.9992415459466));
#29137=CARTESIAN_POINT('Ctrl Pts',(34.1244680994071,-72.5530128872092,26.999062918556));
#29138=CARTESIAN_POINT('Ctrl Pts',(34.1365221810635,-72.5586120395387,26.9988649100354));
#29139=CARTESIAN_POINT('Ctrl Pts',(34.1494625299636,-72.5646260341558,26.9986206326567));
#29140=CARTESIAN_POINT('Ctrl Pts',(34.163106332895,-72.5709691128917,26.9983201877487));
#29141=CARTESIAN_POINT('Ctrl Pts',(34.1798085686584,-72.578734073808,26.9979523942742));
#29142=CARTESIAN_POINT('Ctrl Pts',(34.1975634699253,-72.5869914895447,26.997499916619));
#29143=CARTESIAN_POINT('Ctrl Pts',(34.2159606405676,-72.5955484292679,26.9969537393201));
#29144=CARTESIAN_POINT('Ctrl Pts',(34.2348611311504,-72.6043394744671,26.9963926194015));
#29145=CARTESIAN_POINT('Ctrl Pts',(34.2544339880504,-72.6134440505946,26.9957325028427));
#29146=CARTESIAN_POINT('Ctrl Pts',(34.2742231414687,-72.6226474512814,26.9949774589251));
#29147=CARTESIAN_POINT('Ctrl Pts',(34.2900236652418,-72.6299958480658,26.9943745989079));
#29148=CARTESIAN_POINT('Ctrl Pts',(34.3059607360667,-72.6374066137588,26.993711612265));
#29149=CARTESIAN_POINT('Ctrl Pts',(34.3218342018758,-72.644785372866,26.9929960468146));
#29150=CARTESIAN_POINT('Ctrl Pts',(34.3360016106727,-72.6513710736792,26.9923573892978));
#29151=CARTESIAN_POINT('Ctrl Pts',(34.3501178623903,-72.6579310555955,26.9916770268009));
#29152=CARTESIAN_POINT('Ctrl Pts',(34.3640796025327,-72.6644163574706,26.9909618577939));
#29153=CARTESIAN_POINT('Ctrl Pts',(34.3770874324976,-72.6704585630411,26.9902955513919));
#29154=CARTESIAN_POINT('Ctrl Pts',(34.389960814589,-72.6764358005933,26.9895991550423));
#29155=CARTESIAN_POINT('Ctrl Pts',(34.4026575542914,-72.6823276467199,26.9888776407891));
#29156=CARTESIAN_POINT('Ctrl Pts',(34.4147137119833,-72.6879222345956,26.9881925287195));
#29157=CARTESIAN_POINT('Ctrl Pts',(34.4266103549825,-72.6934397254313,26.9874848652868));
#29158=CARTESIAN_POINT('Ctrl Pts',(34.4383541181474,-72.6988823143506,26.9867568143575));
#29159=CARTESIAN_POINT('Ctrl Pts',(34.4496271379255,-72.7041067395769,26.9860579470175));
#29160=CARTESIAN_POINT('Ctrl Pts',(34.4607590909511,-72.7092620662248,26.9853403733255));
#29161=CARTESIAN_POINT('Ctrl Pts',(34.4717994954728,-72.7143701921677,26.9846027821306));
#29162=CARTESIAN_POINT('Ctrl Pts',(34.4830516132264,-72.7195762726604,26.9838510467243));
#29163=CARTESIAN_POINT('Ctrl Pts',(34.494208022994,-72.7247330573083,26.9830786440325));
#29164=CARTESIAN_POINT('Ctrl Pts',(34.5053743623492,-72.7298878885211,26.9822791770484));
#29165=CARTESIAN_POINT('Ctrl Pts',(34.5161068521514,-72.7348424373365,26.981510772025));
#29166=CARTESIAN_POINT('Ctrl Pts',(34.5268564287903,-72.7397987793137,26.9807167793456));
#29167=CARTESIAN_POINT('Ctrl Pts',(34.5377063841563,-72.7447940225827,26.9798904981477));
#29168=CARTESIAN_POINT('Ctrl Pts',(34.5489423003185,-72.7499669594922,26.9790348240041));
#29169=CARTESIAN_POINT('Ctrl Pts',(34.5602856719162,-72.7551815188518,26.9781444707592));
#29170=CARTESIAN_POINT('Ctrl Pts',(34.5717785652466,-72.7604559078742,26.9772145138921));
#29171=CARTESIAN_POINT('Ctrl Pts',(34.5840671780162,-72.766095473337,26.9762201707355));
#29172=CARTESIAN_POINT('Ctrl Pts',(34.5965266886173,-72.7718034060858,26.9751804717666));
#29173=CARTESIAN_POINT('Ctrl Pts',(34.6091533215573,-72.7775769562531,26.974093291945));
#29174=CARTESIAN_POINT('Ctrl Pts',(34.6225448421687,-72.7837002526563,26.9729402536759));
#29175=CARTESIAN_POINT('Ctrl Pts',(34.6361240193327,-72.789897187906,26.9717337257247));
#29176=CARTESIAN_POINT('Ctrl Pts',(34.649829260066,-72.7961388946458,26.9704767101447));
#29177=CARTESIAN_POINT('Ctrl Pts',(34.6647111637454,-72.8029164828914,26.9691117735377));
#29178=CARTESIAN_POINT('Ctrl Pts',(34.6797412183778,-72.8097466039824,26.967687199764));
#29179=CARTESIAN_POINT('Ctrl Pts',(34.6947812708973,-72.8165662126057,26.9662147977143));
#29180=CARTESIAN_POINT('Ctrl Pts',(34.7121784708218,-72.8244546222023,26.9645116339259));
#29181=CARTESIAN_POINT('Ctrl Pts',(34.7295881416525,-72.83232847794,26.9627442813414));
#29182=CARTESIAN_POINT('Ctrl Pts',(34.7467301342148,-72.8400621253298,26.9609441299777));
#29183=CARTESIAN_POINT('Ctrl Pts',(34.7690864666648,-72.8501482335504,26.9585963992689));
#29184=CARTESIAN_POINT('Ctrl Pts',(34.7909822100655,-72.8599932152628,26.9561926445279));
#29185=CARTESIAN_POINT('Ctrl Pts',(34.8117335912673,-72.8692963615804,26.9538294938965));
#29186=CARTESIAN_POINT('Ctrl Pts',(34.8263877334338,-72.8758660268672,26.9521606919515));
#29187=CARTESIAN_POINT('Ctrl Pts',(34.8404692081152,-72.8821647678184,26.9505129508526));
#29188=CARTESIAN_POINT('Ctrl Pts',(34.8537584983512,-72.8880981139686,26.9489236880989));
#29189=CARTESIAN_POINT('Ctrl Pts',(34.8656824913596,-72.8934218879817,26.9474977008846));
#29190=CARTESIAN_POINT('Ctrl Pts',(34.8769680122958,-72.8984512256775,26.9461190319871));
#29191=CARTESIAN_POINT('Ctrl Pts',(34.8874906704523,-72.9031338368634,26.9448124824959));
#29192=CARTESIAN_POINT('Ctrl Pts',(34.8973142788575,-72.9075053690295,26.9435927307589));
#29193=CARTESIAN_POINT('Ctrl Pts',(34.9064725793694,-72.9115745492444,26.9424359792807));
#29194=CARTESIAN_POINT('Ctrl Pts',(34.9149034806463,-72.9153163971448,26.9413577939785));
#29195=CARTESIAN_POINT('Ctrl Pts',(34.9229180225557,-72.9188734541938,26.940332854769));
#29196=CARTESIAN_POINT('Ctrl Pts',(34.9302749193298,-72.9221345908904,26.9393790077743));
#29197=CARTESIAN_POINT('Ctrl Pts',(34.9369627380912,-72.9250967827356,26.9385036410478));
#29198=CARTESIAN_POINT('Ctrl Pts',(34.9433872602677,-72.9279423543456,26.9376627371377));
#29199=CARTESIAN_POINT('Ctrl Pts',(34.9491941014795,-72.9305119583031,26.9368943156628));
#29200=CARTESIAN_POINT('Ctrl Pts',(34.9544168588578,-72.9328219368754,26.9361981656302));
#29201=CARTESIAN_POINT('Ctrl Pts',(34.9593918014892,-72.9350223092159,26.9355350472381));
#29202=CARTESIAN_POINT('Ctrl Pts',(34.9638366931368,-72.9369870780134,26.9349375205311));
#29203=CARTESIAN_POINT('Ctrl Pts',(34.9678232367822,-72.9387488347673,26.9343986405426));
#29204=CARTESIAN_POINT('Ctrl Pts',(34.9717196612948,-72.9404707655454,26.9338719423841));
#29205=CARTESIAN_POINT('Ctrl Pts',(34.9751780232743,-72.941998670718,26.933401294822));
#29206=CARTESIAN_POINT('Ctrl Pts',(34.9783093387544,-72.9433820368175,26.9329732619374));
#29207=CARTESIAN_POINT('Ctrl Pts',(34.9813422498734,-72.9447219294127,26.9325586803651));
#29208=CARTESIAN_POINT('Ctrl Pts',(34.9840682614716,-72.9459261859505,26.9321840818727));
#29209=CARTESIAN_POINT('Ctrl Pts',(34.9866320307011,-72.9470587250239,26.9318304705446));
#29210=CARTESIAN_POINT('Ctrl Pts',(34.988787344238,-72.9480108297485,26.9315331960187));
#29211=CARTESIAN_POINT('Ctrl Pts',(34.9908286451645,-72.9489125305568,26.9312506527497));
#29212=CARTESIAN_POINT('Ctrl Pts',(34.9928678625178,-72.9498130615485,26.9309675781304));
#29213=CARTESIAN_POINT('Ctrl Pts',(35.4109431177646,-72.046685660721,26.9968209210375));
#29214=CARTESIAN_POINT('Ctrl Pts',(35.271584699349,-72.3477281276635,26.9748698067351));
#29215=CARTESIAN_POINT('Ctrl Pts',(35.1322262809334,-72.648770594606,26.9529186924328));
#29216=CARTESIAN_POINT('Ctrl Pts',(34.9928678625178,-72.9498130615485,26.9309675781304));
#29217=CARTESIAN_POINT('',(34.6048809642881,-72.2245134174903,27.));
#29218=CARTESIAN_POINT('Ctrl Pts',(42.196820839876,-72.0466869074717,20.2109458098101));
#29219=CARTESIAN_POINT('Ctrl Pts',(42.1968651977585,-72.0460055194057,20.2094745117698));
#29220=CARTESIAN_POINT('Ctrl Pts',(42.1969518986639,-72.0445752373298,20.2063859972174));
#29221=CARTESIAN_POINT('Ctrl Pts',(42.1975052069546,-72.0362666836179,20.1884462883035));
#29222=CARTESIAN_POINT('Ctrl Pts',(42.1987929121607,-72.0112744135499,20.1344729899145));
#29223=CARTESIAN_POINT('Ctrl Pts',(42.1996557821269,-71.9844303509257,20.0764815416121));
#29224=CARTESIAN_POINT('Ctrl Pts',(42.2000060028006,-71.9594532548772,20.022522027641));
#29225=CARTESIAN_POINT('Ctrl Pts',(42.1999927639906,-71.9511381376986,20.004560090378));
#29226=CARTESIAN_POINT('Ctrl Pts',(42.2,-71.9497084248624,20.0014721226316));
#29227=CARTESIAN_POINT('Ctrl Pts',(42.2,-71.9490268349807,20.));
#29228=CARTESIAN_POINT('Ctrl Pts',(42.1748696276389,-72.3477293564499,20.0715873944326));
#29229=CARTESIAN_POINT('Ctrl Pts',(42.1750195593748,-72.3462468301403,20.0683107887067));
#29230=CARTESIAN_POINT('Ctrl Pts',(42.1755112872819,-72.342363439581,20.0597605016236));
#29231=CARTESIAN_POINT('Ctrl Pts',(42.1782699776807,-72.3223182757032,20.0159145750237));
#29232=CARTESIAN_POINT('Ctrl Pts',(42.1845158453337,-72.2729887945663,19.9085740298018));
#29233=CARTESIAN_POINT('Ctrl Pts',(42.1930982717819,-72.207684249358,19.7663902797076));
#29234=CARTESIAN_POINT('Ctrl Pts',(42.1980895940111,-72.1582938438831,19.6590311049478));
#29235=CARTESIAN_POINT('Ctrl Pts',(42.1997838820197,-72.1381225623237,19.6151120158836));
#29236=CARTESIAN_POINT('Ctrl Pts',(42.2,-72.1341926423635,19.6065422105412));
#29237=CARTESIAN_POINT('Ctrl Pts',(42.2,-72.1326845566538,19.6032539761921));
#29238=CARTESIAN_POINT('Ctrl Pts',(42.1529184154018,-72.6487718054281,19.9322289790551));
#29239=CARTESIAN_POINT('Ctrl Pts',(42.1533738444073,-72.6464941085306,19.9271284658077));
#29240=CARTESIAN_POINT('Ctrl Pts',(42.1544898154414,-72.6425808645548,19.9181056666025));
#29241=CARTESIAN_POINT('Ctrl Pts',(42.162296347732,-72.6159506839129,19.8602311090506));
#29242=CARTESIAN_POINT('Ctrl Pts',(42.1782299355538,-72.5231682072857,19.6622832801377));
#29243=CARTESIAN_POINT('Ctrl Pts',(42.1937530235431,-72.4384015430389,19.4764686505132));
#29244=CARTESIAN_POINT('Ctrl Pts',(42.1979624296397,-72.3480974306778,19.2786157337193));
#29245=CARTESIAN_POINT('Ctrl Pts',(42.1994067391489,-72.3226741649949,19.2206367291843));
#29246=CARTESIAN_POINT('Ctrl Pts',(42.2,-72.3186768598647,19.2116122984507));
#29247=CARTESIAN_POINT('Ctrl Pts',(42.2,-72.3163422783269,19.2065079523841));
#29248=CARTESIAN_POINT('Ctrl Pts',(42.1309672031646,-72.9498142544064,19.7928705636776));
#29249=CARTESIAN_POINT('Ctrl Pts',(42.1319235023647,-72.9467720369169,19.7859815787116));
#29250=CARTESIAN_POINT('Ctrl Pts',(42.1337967255951,-72.9403552446875,19.7715258643937));
#29251=CARTESIAN_POINT('Ctrl Pts',(42.145647611726,-72.9035152339706,19.6878058974393));
#29252=CARTESIAN_POINT('Ctrl Pts',(42.1734427243359,-72.7907453606573,19.4364956174772));
#29253=CARTESIAN_POINT('Ctrl Pts',(42.1924901231468,-72.6655771656199,19.1664440243787));
#29254=CARTESIAN_POINT('Ctrl Pts',(42.2001344088158,-72.5485935297578,18.9151457627271));
#29255=CARTESIAN_POINT('Ctrl Pts',(42.1998426456441,-72.5097905257285,18.8311910575127));
#29256=CARTESIAN_POINT('Ctrl Pts',(42.2,-72.5031610773659,18.8166823863602));
#29257=CARTESIAN_POINT('Ctrl Pts',(42.2,-72.5,18.8097619285762));
#29258=CARTESIAN_POINT('Ctrl Pts',(42.1309672031646,-72.9498142544064,19.7928705636776));
#29259=CARTESIAN_POINT('Ctrl Pts',(42.1529184154018,-72.6487718054281,19.9322289790551));
#29260=CARTESIAN_POINT('Ctrl Pts',(42.1748696276389,-72.3477293564499,20.0715873944326));
#29261=CARTESIAN_POINT('Ctrl Pts',(42.196820839876,-72.0466869074717,20.2109458098101));
#29262=CARTESIAN_POINT('Ctrl Pts',(42.1309672031646,-72.9498142544064,19.7928705636776));
#29263=CARTESIAN_POINT('Ctrl Pts',(42.0459074091364,-73.2204098933174,20.4056240222309));
#29264=CARTESIAN_POINT('Ctrl Pts',(41.704007781412,-73.7466614991037,21.7070010142552));
#29265=CARTESIAN_POINT('Ctrl Pts',(41.0578917243185,-74.000000000005,22.9273203194824));
#29266=CARTESIAN_POINT('Ctrl Pts',(40.699999999979,-74.,23.4706975310694));
#29267=CARTESIAN_POINT('Ctrl Pts',(42.1529184154018,-72.6487718054281,19.9322289790551));
#29268=CARTESIAN_POINT('Ctrl Pts',(42.0900566190563,-72.9237208747561,20.544894147307));
#29269=CARTESIAN_POINT('Ctrl Pts',(41.7929657367318,-73.4750045131386,21.8418272713667));
#29270=CARTESIAN_POINT('Ctrl Pts',(41.1749647057687,-73.7841592833289,23.0483683735484));
#29271=CARTESIAN_POINT('Ctrl Pts',(40.8245617157746,-73.8157835059031,23.5830861153787));
#29272=CARTESIAN_POINT('Ctrl Pts',(42.1748696276389,-72.3477293564499,20.0715873944326));
#29273=CARTESIAN_POINT('Ctrl Pts',(42.1342058289762,-72.6270318561947,20.6841642723831));
#29274=CARTESIAN_POINT('Ctrl Pts',(41.8819236920516,-73.2033475271735,21.9766535284783));
#29275=CARTESIAN_POINT('Ctrl Pts',(41.2920376872189,-73.5683185666529,23.1694164276145));
#29276=CARTESIAN_POINT('Ctrl Pts',(40.9491234315702,-73.6315670118063,23.6954746996879));
#29277=CARTESIAN_POINT('Ctrl Pts',(42.196820839876,-72.0466869074717,20.2109458098101));
#29278=CARTESIAN_POINT('Ctrl Pts',(42.1783550388962,-72.3303428376334,20.8234343974591));
#29279=CARTESIAN_POINT('Ctrl Pts',(41.9708816473713,-72.9316905412085,22.1114797855899));
#29280=CARTESIAN_POINT('Ctrl Pts',(41.409110668669,-73.3524778499768,23.2904644816805));
#29281=CARTESIAN_POINT('Ctrl Pts',(41.0736851473658,-73.4473505177094,23.8078632839972));
#29282=CARTESIAN_POINT('',(41.0736851473658,-73.4473505177094,23.8078632839972));
#29283=CARTESIAN_POINT('Origin',(35.2,-73.75,20.));
#29284=CARTESIAN_POINT('',(39.5301270189222,-73.5,25.5));
#29285=CARTESIAN_POINT('',(40.3071428571429,-74.,24.0208322318563));
#29286=CARTESIAN_POINT('Ctrl Pts',(40.699999999979,-74.,23.4706975310694));
#29287=CARTESIAN_POINT('Ctrl Pts',(40.5730966676381,-74.,23.6633713879345));
#29288=CARTESIAN_POINT('Ctrl Pts',(40.4446625272125,-74.,23.8461587910824));
#29289=CARTESIAN_POINT('Ctrl Pts',(40.3071428571429,-74.,24.0208322318563));
#29290=CARTESIAN_POINT('Ctrl Pts',(40.8245617157746,-73.8157835059031,23.5830861153787));
#29291=CARTESIAN_POINT('Ctrl Pts',(40.7003137824799,-73.8269970069562,23.7726894470159));
#29292=CARTESIAN_POINT('Ctrl Pts',(40.5728443653613,-73.8333333333333,23.9527761154313));
#29293=CARTESIAN_POINT('Ctrl Pts',(40.4380952380953,-73.8333333333333,24.1239304942116));
#29294=CARTESIAN_POINT('Ctrl Pts',(40.9491234315702,-73.6315670118063,23.6954746996879));
#29295=CARTESIAN_POINT('Ctrl Pts',(40.8275308973216,-73.6539940139125,23.8820075060973));
#29296=CARTESIAN_POINT('Ctrl Pts',(40.7010262035101,-73.6666666666667,24.0593934397802));
#29297=CARTESIAN_POINT('Ctrl Pts',(40.5690476190476,-73.6666666666667,24.2270287565669));
#29298=CARTESIAN_POINT('Ctrl Pts',(41.0736851473658,-73.4473505177094,23.8078632839972));
#29299=CARTESIAN_POINT('Ctrl Pts',(40.9547480121633,-73.4809910208687,23.9913255651787));
#29300=CARTESIAN_POINT('Ctrl Pts',(40.8292080416589,-73.5,24.1660107641291));
#29301=CARTESIAN_POINT('Ctrl Pts',(40.7,-73.5,24.3301270189222));
#29302=CARTESIAN_POINT('Ctrl Pts',(38.670697532745,-74.,25.4999999988754));
#29303=CARTESIAN_POINT('Ctrl Pts',(38.3480203762685,-74.0000000001593,25.7125291250959));
#29304=CARTESIAN_POINT('Ctrl Pts',(37.8159361986621,-73.9255312874326,26.0143563494905));
#29305=CARTESIAN_POINT('Ctrl Pts',(36.6753333677337,-73.6438750005303,26.5487153899226));
#29306=CARTESIAN_POINT('Ctrl Pts',(35.6787076842961,-73.2526841673963,26.8357625004906));
#29307=CARTESIAN_POINT('Ctrl Pts',(34.9928678625178,-72.9498130615485,26.9309675781304));
#29308=CARTESIAN_POINT('Ctrl Pts',(38.7830861170276,-73.8157835060006,25.6245617146941));
#29309=CARTESIAN_POINT('Ctrl Pts',(38.4655512687303,-73.7970038922842,25.8326437580241));
#29310=CARTESIAN_POINT('Ctrl Pts',(37.9402230267678,-73.6962906722935,26.1238795687314));
#29311=CARTESIAN_POINT('Ctrl Pts',(36.8104945847949,-73.3693647115943,26.6290704767058));
#29312=CARTESIAN_POINT('Ctrl Pts',(35.8179633331108,-72.956512531518,26.8825594092965));
#29313=CARTESIAN_POINT('Ctrl Pts',(35.1322262809334,-72.648770594606,26.9529186924328));
#29314=CARTESIAN_POINT('Ctrl Pts',(38.8954747013101,-73.6315670120013,25.7491234305128));
#29315=CARTESIAN_POINT('Ctrl Pts',(38.5830821611921,-73.5940077844089,25.9527583909524));
#29316=CARTESIAN_POINT('Ctrl Pts',(38.0645098548735,-73.4670500571544,26.2334027879723));
#29317=CARTESIAN_POINT('Ctrl Pts',(36.9456558018562,-73.0948544226583,26.7094255634889));
#29318=CARTESIAN_POINT('Ctrl Pts',(35.9572189819256,-72.6603408956398,26.9293563181024));
#29319=CARTESIAN_POINT('Ctrl Pts',(35.271584699349,-72.3477281276635,26.9748698067351));
#29320=CARTESIAN_POINT('Ctrl Pts',(39.0078632855927,-73.4473505180019,25.8736851463315));
#29321=CARTESIAN_POINT('Ctrl Pts',(38.7006130536539,-73.3910116765338,26.0728730238806));
#29322=CARTESIAN_POINT('Ctrl Pts',(38.1887966829792,-73.2378094420153,26.3429260072132));
#29323=CARTESIAN_POINT('Ctrl Pts',(37.0808170189174,-72.8203441337222,26.7897806502721));
#29324=CARTESIAN_POINT('Ctrl Pts',(36.0964746307403,-72.3641692597616,26.9761532269083));
#29325=CARTESIAN_POINT('Ctrl Pts',(35.4109431177646,-72.046685660721,26.9968209210375));
#29326=CARTESIAN_POINT('Ctrl Pts',(34.9928678625178,-72.9498130615485,26.9309675781304));
#29327=CARTESIAN_POINT('Ctrl Pts',(35.6787076842961,-73.2526841673963,26.8357625004906));
#29328=CARTESIAN_POINT('Ctrl Pts',(36.6753333677337,-73.6438750005303,26.5487153899226));
#29329=CARTESIAN_POINT('Ctrl Pts',(37.8159361986621,-73.9255312874326,26.0143563494905));
#29330=CARTESIAN_POINT('Ctrl Pts',(38.3480203762685,-74.0000000001593,25.7125291250959));
#29331=CARTESIAN_POINT('Ctrl Pts',(38.670697532745,-74.,25.4999999988754));
#29332=CARTESIAN_POINT('',(38.6706975330488,-74.,25.4999999993376));
#29333=CARTESIAN_POINT('Ctrl Pts',(39.2208322318563,-74.,25.1071428571429));
#29334=CARTESIAN_POINT('Ctrl Pts',(39.0524411521674,-74.,25.2397164505804));
#29335=CARTESIAN_POINT('Ctrl Pts',(38.8678098322883,-74.,25.3701733162485));
#29336=CARTESIAN_POINT('Ctrl Pts',(38.6706975327445,-74.,25.4999999988757));
#29337=CARTESIAN_POINT('Ctrl Pts',(39.3239304942116,-73.8333333333333,25.2380952380952));
#29338=CARTESIAN_POINT('Ctrl Pts',(39.1589319088021,-73.8333333333333,25.3679979349617));
#29339=CARTESIAN_POINT('Ctrl Pts',(38.9770571586008,-73.8272553216869,25.4974516009823));
#29340=CARTESIAN_POINT('Ctrl Pts',(38.7830861170271,-73.8157835060006,25.6245617146944));
#29341=CARTESIAN_POINT('Ctrl Pts',(39.4270287565669,-73.6666666666667,25.3690476190476));
#29342=CARTESIAN_POINT('Ctrl Pts',(39.2654226654369,-73.6666666666667,25.496279419343));
#29343=CARTESIAN_POINT('Ctrl Pts',(39.0863044849134,-73.6545106433737,25.6247298857161));
#29344=CARTESIAN_POINT('Ctrl Pts',(38.8954747013097,-73.6315670120012,25.7491234305131));
#29345=CARTESIAN_POINT('Ctrl Pts',(39.5301270189222,-73.5,25.5));
#29346=CARTESIAN_POINT('Ctrl Pts',(39.3719134220716,-73.5,25.6245609037243));
#29347=CARTESIAN_POINT('Ctrl Pts',(39.195551811226,-73.4817659650606,25.75200817045));
#29348=CARTESIAN_POINT('Ctrl Pts',(39.0078632855922,-73.4473505180018,25.8736851463318));
#29349=CARTESIAN_POINT('Origin',(25.2,-72.5,25.5));
#29350=CARTESIAN_POINT('',(25.2,-72.5,27.));
#29351=CARTESIAN_POINT('Origin',(35.2,-32.,27.));
#29352=CARTESIAN_POINT('Origin',(35.2,-72.,4.));
#29353=CARTESIAN_POINT('',(35.2,-72.,4.));
#29354=CARTESIAN_POINT('Origin',(28.2,-72.,3.99999999999999));
#29355=CARTESIAN_POINT('',(28.2,-72.,11.));
#29356=CARTESIAN_POINT('Origin',(2.2,-72.,11.));
#29357=CARTESIAN_POINT('',(2.2,-72.,11.));
#29358=CARTESIAN_POINT('Origin',(2.2,-72.,4.));
#29359=CARTESIAN_POINT('Origin',(-7.1,-32.,-4.));
#29360=CARTESIAN_POINT('',(-7.1,-32.,4.));
#29361=CARTESIAN_POINT('',(-7.1,-32.,-4.));
#29362=CARTESIAN_POINT('Origin',(2.20000000000001,-32.,-3.99999999999999));
#29363=CARTESIAN_POINT('',(2.2,-32.,-13.3));
#29364=CARTESIAN_POINT('Origin',(28.2,-32.,-13.3));
#29365=CARTESIAN_POINT('Origin',(2.2,-32.,3.99999999999999));
#29366=CARTESIAN_POINT('',(0.,0.,0.));
#29367=CARTESIAN_POINT('Origin',(25.7,-73.75,-60.25));
#29368=CARTESIAN_POINT('',(-5.8,-73.5,-60.5));
#29369=CARTESIAN_POINT('',(-5.8,-74.,-60.));
#29370=CARTESIAN_POINT('',(-5.8,-73.5,-60.5));
#29371=CARTESIAN_POINT('',(6.7,-74.,-60.));
#29372=CARTESIAN_POINT('',(25.7,-74.,-60.));
#29373=CARTESIAN_POINT('',(23.7,-74.,-60.));
#29374=CARTESIAN_POINT('',(15.2,-74.,-60.));
#29375=CARTESIAN_POINT('',(36.2,-74.,-60.));
#29376=CARTESIAN_POINT('',(25.7,-74.,-60.));
#29377=CARTESIAN_POINT('',(36.2,-73.5,-60.5));
#29378=CARTESIAN_POINT('',(36.2,-74.,-60.));
#29379=CARTESIAN_POINT('',(25.7,-73.5,-60.5));
#29380=CARTESIAN_POINT('Origin',(-5.8,-69.,-60.25));
#29381=CARTESIAN_POINT('',(-10.3,-69.,-60.5));
#29382=CARTESIAN_POINT('',(-10.8,-69.,-60.));
#29383=CARTESIAN_POINT('',(-10.3,-69.,-60.5));
#29384=CARTESIAN_POINT('Origin',(-5.8,-69.,-60.));
#29385=CARTESIAN_POINT('Origin',(-5.8,-69.,-60.5));
#29386=CARTESIAN_POINT('Origin',(-10.55,-61.,-60.25));
#29387=CARTESIAN_POINT('',(-10.3,-37.,-60.5));
#29388=CARTESIAN_POINT('',(-10.8,-37.,-60.));
#29389=CARTESIAN_POINT('',(-10.3,-37.,-60.5));
#29390=CARTESIAN_POINT('',(-10.8,-61.,-60.));
#29391=CARTESIAN_POINT('',(-10.3,-61.,-60.5));
#29392=CARTESIAN_POINT('Origin',(-5.79999999999999,-37.,-60.25));
#29393=CARTESIAN_POINT('',(-5.8,-32.5,-60.5));
#29394=CARTESIAN_POINT('',(-5.8,-32.,-60.));
#29395=CARTESIAN_POINT('',(-5.8,-32.5,-60.5));
#29396=CARTESIAN_POINT('Origin',(-5.79999999999999,-37.,-60.));
#29397=CARTESIAN_POINT('Origin',(-5.79999999999999,-37.,-60.5));
#29398=CARTESIAN_POINT('Origin',(4.7,-32.25,-60.25));
#29399=CARTESIAN_POINT('',(36.2,-32.5,-60.5));
#29400=CARTESIAN_POINT('',(36.2,-32.,-60.));
#29401=CARTESIAN_POINT('',(36.2,-32.5,-60.5));
#29402=CARTESIAN_POINT('',(4.7,-32.,-60.));
#29403=CARTESIAN_POINT('',(4.7,-32.5,-60.5));
#29404=CARTESIAN_POINT('Origin',(36.2,-37.,-60.25));
#29405=CARTESIAN_POINT('',(40.7,-37.,-60.5));
#29406=CARTESIAN_POINT('',(41.2,-37.,-60.));
#29407=CARTESIAN_POINT('',(40.7,-37.,-60.5));
#29408=CARTESIAN_POINT('Origin',(36.2,-37.,-60.));
#29409=CARTESIAN_POINT('Origin',(36.2,-37.,-60.5));
#29410=CARTESIAN_POINT('Origin',(40.95,-45.,-60.25));
#29411=CARTESIAN_POINT('',(40.7,-69.,-60.5));
#29412=CARTESIAN_POINT('',(41.2,-69.,-60.));
#29413=CARTESIAN_POINT('',(40.7,-69.,-60.5));
#29414=CARTESIAN_POINT('',(41.2,-45.,-60.));
#29415=CARTESIAN_POINT('',(40.7,-45.,-60.5));
#29416=CARTESIAN_POINT('Origin',(36.2,-69.,-60.25));
#29417=CARTESIAN_POINT('Origin',(36.2,-69.,-60.));
#29418=CARTESIAN_POINT('Origin',(36.2,-69.,-60.5));
#29419=CARTESIAN_POINT('Origin',(15.2,-53.,-60.));
#29420=CARTESIAN_POINT('',(24.2,-74.5,-60.));
#29421=CARTESIAN_POINT('',(16.45,-66.7499999999999,-60.));
#29422=CARTESIAN_POINT('',(24.2,-75.5,-60.));
#29423=CARTESIAN_POINT('',(24.2,-63.5,-60.));
#29424=CARTESIAN_POINT('',(36.2,-75.5,-60.));
#29425=CARTESIAN_POINT('',(4.7,-75.5,-60.));
#29426=CARTESIAN_POINT('',(42.7,-69.,-60.));
#29427=CARTESIAN_POINT('Origin',(36.2,-69.,-60.));
#29428=CARTESIAN_POINT('',(42.7,-37.,-60.));
#29429=CARTESIAN_POINT('',(42.7,-61.,-60.));
#29430=CARTESIAN_POINT('',(36.2,-30.5,-60.));
#29431=CARTESIAN_POINT('Origin',(36.2,-37.,-60.));
#29432=CARTESIAN_POINT('',(-5.8,-30.5,-60.));
#29433=CARTESIAN_POINT('',(25.7,-30.5,-60.));
#29434=CARTESIAN_POINT('',(-12.3,-37.,-60.));
#29435=CARTESIAN_POINT('Origin',(-5.79999999999999,-37.,-60.));
#29436=CARTESIAN_POINT('',(-12.3,-69.,-60.));
#29437=CARTESIAN_POINT('',(-12.3,-45.,-60.));
#29438=CARTESIAN_POINT('',(-5.8,-75.5,-60.));
#29439=CARTESIAN_POINT('Origin',(-5.8,-69.,-60.));
#29440=CARTESIAN_POINT('',(6.2,-75.5,-60.));
#29441=CARTESIAN_POINT('',(4.7,-75.5,-60.));
#29442=CARTESIAN_POINT('',(6.2,-74.5,-60.));
#29443=CARTESIAN_POINT('',(6.2,-63.5,-60.));
#29444=CARTESIAN_POINT('',(13.95,-66.7499999999999,-60.));
#29445=CARTESIAN_POINT('Origin',(-5.79999999999999,-37.,-60.));
#29446=CARTESIAN_POINT('',(-10.3,-37.,-79.5));
#29447=CARTESIAN_POINT('',(-10.3,-37.,-60.));
#29448=CARTESIAN_POINT('',(-5.8,-32.5,-79.5));
#29449=CARTESIAN_POINT('Origin',(-5.79999999999999,-37.,-79.5));
#29450=CARTESIAN_POINT('',(-5.8,-32.5,-60.));
#29451=CARTESIAN_POINT('Origin',(-10.3,-69.,-60.));
#29452=CARTESIAN_POINT('',(-10.3,-69.,-79.5));
#29453=CARTESIAN_POINT('',(-10.3,-69.,-60.));
#29454=CARTESIAN_POINT('',(-10.3,-37.,-79.5));
#29455=CARTESIAN_POINT('Origin',(-5.8,-69.,-60.));
#29456=CARTESIAN_POINT('',(-5.8,-73.5,-79.5));
#29457=CARTESIAN_POINT('',(-5.8,-73.5,-60.));
#29458=CARTESIAN_POINT('Origin',(-5.8,-69.,-79.5));
#29459=CARTESIAN_POINT('Origin',(36.2,-73.5,-60.));
#29460=CARTESIAN_POINT('',(36.2,-73.5,-79.5));
#29461=CARTESIAN_POINT('',(36.2,-73.5,-60.));
#29462=CARTESIAN_POINT('',(-5.8,-73.5,-79.5));
#29463=CARTESIAN_POINT('Origin',(23.7,-74.5,-12.));
#29464=CARTESIAN_POINT('',(23.7,-74.,-12.5));
#29465=CARTESIAN_POINT('',(24.2,-74.5,-12.5));
#29466=CARTESIAN_POINT('',(23.7,-74.,-12.5));
#29467=CARTESIAN_POINT('',(23.7,-74.5,-12.));
#29468=CARTESIAN_POINT('',(23.7,-74.5,-12.));
#29469=CARTESIAN_POINT('',(24.2,-74.5,-12.5));
#29470=CARTESIAN_POINT('Origin',(19.7,-74.25,-12.25));
#29471=CARTESIAN_POINT('',(6.45,-74.25,-12.25));
#29472=CARTESIAN_POINT('',(6.7,-74.5,-12.));
#29473=CARTESIAN_POINT('',(8.61666666666665,-76.4166666666667,-10.0833333333334));
#29474=CARTESIAN_POINT('',(19.7,-74.5,-12.));
#29475=CARTESIAN_POINT('',(6.7,-74.,-12.5));
#29476=CARTESIAN_POINT('',(19.7,-74.,-12.5));
#29477=CARTESIAN_POINT('',(10.8666666666666,-69.8333333333333,-16.6666666666666));
#29478=CARTESIAN_POINT('Origin',(23.95,-74.,-12.25));
#29479=CARTESIAN_POINT('',(23.95,-75.75,-12.25));
#29480=CARTESIAN_POINT('',(24.2,-75.5,-12.5));
#29481=CARTESIAN_POINT('',(34.5333333333335,-65.1666666666667,-22.8333333333335));
#29482=CARTESIAN_POINT('',(24.2,-74.,-12.5));
#29483=CARTESIAN_POINT('',(23.7,-75.5,-12.));
#29484=CARTESIAN_POINT('',(23.7,-74.,-12.));
#29485=CARTESIAN_POINT('',(21.2,-73.,-9.49999999999997));
#29486=CARTESIAN_POINT('Origin',(23.95,-74.25,-52.5));
#29487=CARTESIAN_POINT('',(23.7,-74.,-52.5));
#29488=CARTESIAN_POINT('',(24.2,-74.5,-52.5));
#29489=CARTESIAN_POINT('Origin',(24.2,-74.,-12.));
#29490=CARTESIAN_POINT('',(6.7,-75.5,-12.));
#29491=CARTESIAN_POINT('',(6.7,-74.,-12.));
#29492=CARTESIAN_POINT('',(9.2,-75.5,-12.));
#29493=CARTESIAN_POINT('Origin',(6.45,-74.,-12.25));
#29494=CARTESIAN_POINT('',(6.2,-74.5,-12.5));
#29495=CARTESIAN_POINT('',(4.28333333333335,-76.4166666666667,-14.4166666666666));
#29496=CARTESIAN_POINT('',(6.2,-75.5,-12.5));
#29497=CARTESIAN_POINT('',(6.2,-74.,-12.5));
#29498=CARTESIAN_POINT('',(6.2,-75.5,-12.5));
#29499=CARTESIAN_POINT('Origin',(6.45,-74.25,-25.5));
#29500=CARTESIAN_POINT('',(6.7,-74.,-25.5));
#29501=CARTESIAN_POINT('',(6.2,-74.5,-25.5));
#29502=CARTESIAN_POINT('Origin',(15.2,-74.,-39.));
#29503=CARTESIAN_POINT('Ctrl Pts',(-5.56630111765684,-30.048846456053,-80.4393174796692));
#29504=CARTESIAN_POINT('Ctrl Pts',(-5.55472999163838,-30.0474878607419,
-80.4332835106634));
#29505=CARTESIAN_POINT('Ctrl Pts',(-5.50914704734725,-30.0412161151931,
-80.4097058743082));
#29506=CARTESIAN_POINT('Ctrl Pts',(-5.26592539574766,-30.018413630151,-80.2818322468851));
#29507=CARTESIAN_POINT('Ctrl Pts',(-5.03984528472998,-30.0051078595377,
-80.1608659535269));
#29508=CARTESIAN_POINT('Ctrl Pts',(-4.79674507928722,-29.9990490307073,
-80.0305394911781));
#29509=CARTESIAN_POINT('Ctrl Pts',(-4.75094774329034,-30.,-80.006159003494));
#29510=CARTESIAN_POINT('Ctrl Pts',(-4.73933982822015,-30.,-80.));
#29511=CARTESIAN_POINT('Ctrl Pts',(-5.72305909304156,-30.033897250275,-80.1460536871276));
#29512=CARTESIAN_POINT('Ctrl Pts',(-5.71422864812372,-30.0331851743567,
-80.1414222172682));
#29513=CARTESIAN_POINT('Ctrl Pts',(-5.68538075880276,-30.029214011803,-80.126606885425));
#29514=CARTESIAN_POINT('Ctrl Pts',(-5.48880222005144,-30.0103524135108,
-80.0234452250129));
#29515=CARTESIAN_POINT('Ctrl Pts',(-5.32713234249905,-30.0016369910093,
-79.9366792528958));
#29516=CARTESIAN_POINT('Ctrl Pts',(-5.13072308176098,-29.998410805748,-79.8311710354903));
#29517=CARTESIAN_POINT('Ctrl Pts',(-5.10173254804783,-30.,-79.8157122686222));
#29518=CARTESIAN_POINT('Ctrl Pts',(-5.09289321881343,-30.,-79.8110177634954));
#29519=CARTESIAN_POINT('Ctrl Pts',(-5.87981706842629,-30.018948044497,-79.8527898945859));
#29520=CARTESIAN_POINT('Ctrl Pts',(-5.87375891162897,-30.0186527919516,
-79.8495895275592));
#29521=CARTESIAN_POINT('Ctrl Pts',(-5.8439723661837,-30.0162635432914,-79.8337973075619));
#29522=CARTESIAN_POINT('Ctrl Pts',(-5.727605526545,-30.0100867792541,-79.7718561188082));
#29523=CARTESIAN_POINT('Ctrl Pts',(-5.59851606708718,-30.0033535127243,
-79.7031093748739));
#29524=CARTESIAN_POINT('Ctrl Pts',(-5.48232352746253,-30.000714223928,-79.6411500710076));
#29525=CARTESIAN_POINT('Ctrl Pts',(-5.45251735280532,-30.,-79.6252655337503));
#29526=CARTESIAN_POINT('Ctrl Pts',(-5.44644660940672,-30.,-79.6220355269908));
#29527=CARTESIAN_POINT('Ctrl Pts',(-6.03657504381102,-30.0039988387189,
-79.5595261020443));
#29528=CARTESIAN_POINT('Ctrl Pts',(-6.03327514811522,-30.0038872502628,
-79.5577612253643));
#29529=CARTESIAN_POINT('Ctrl Pts',(-6.02026555880084,-30.0033696172087,
-79.5508019948342));
#29530=CARTESIAN_POINT('Ctrl Pts',(-5.95065272607528,-30.0014965556721,
-79.5135781548536));
#29531=CARTESIAN_POINT('Ctrl Pts',(-5.88593766744229,-30.0004169765915,
-79.4789879704714));
#29532=CARTESIAN_POINT('Ctrl Pts',(-5.81635283613372,-29.9999223146288,
-79.4417957477402));
#29533=CARTESIAN_POINT('Ctrl Pts',(-5.8033021575628,-30.,-79.4348187988785));
#29534=CARTESIAN_POINT('Ctrl Pts',(-5.8,-30.,-79.4330532904862));
#29535=CARTESIAN_POINT('',(-4.73933982822015,-30.,-80.));
#29536=CARTESIAN_POINT('',(-5.56630111765684,-30.048846456053,-80.4393174796692));
#29537=CARTESIAN_POINT('Ctrl Pts',(-4.73933982822015,-30.,-80.));
#29538=CARTESIAN_POINT('Ctrl Pts',(-4.74144196548162,-30.,-80.0011153657362));
#29539=CARTESIAN_POINT('Ctrl Pts',(-4.74354800689035,-30.0000008803716,
-80.0022328244698));
#29540=CARTESIAN_POINT('Ctrl Pts',(-4.74582631569054,-30.000002963202,-80.0034427894735));
#29541=CARTESIAN_POINT('Ctrl Pts',(-4.74816258095287,-30.0000050990163,
-80.0046835340147));
#29542=CARTESIAN_POINT('Ctrl Pts',(-4.75067986365268,-30.0000084969638,
-80.0060214841799));
#29543=CARTESIAN_POINT('Ctrl Pts',(-4.75351150864003,-30.0000141688287,
-80.007528287592));
#29544=CARTESIAN_POINT('Ctrl Pts',(-4.756425520977,-30.0000200056777,-80.0090789211466));
#29545=CARTESIAN_POINT('Ctrl Pts',(-4.75967230457741,-30.0000282443224,
-80.0108082969316));
#29546=CARTESIAN_POINT('Ctrl Pts',(-4.7633488278572,-30.0000407594512,-80.0127685607417));
#29547=CARTESIAN_POINT('Ctrl Pts',(-4.76722661255211,-30.0000539596872,
-80.0148361339413));
#29548=CARTESIAN_POINT('Ctrl Pts',(-4.77158245475638,-30.0000719133563,
-80.0171605566096));
#29549=CARTESIAN_POINT('Ctrl Pts',(-4.77647810826652,-30.0000977659287,
-80.0197750892952));
#29550=CARTESIAN_POINT('Ctrl Pts',(-4.78159298377548,-30.000124776151,-80.022506697889));
#29551=CARTESIAN_POINT('Ctrl Pts',(-4.78729688562401,-30.0001604227472,
-80.0255548684521));
#29552=CARTESIAN_POINT('Ctrl Pts',(-4.79360683616279,-30.0002092303521,
-80.0289288373614));
#29553=CARTESIAN_POINT('Ctrl Pts',(-4.80027903556804,-30.0002608399599,
-80.0324965029417));
#29554=CARTESIAN_POINT('Ctrl Pts',(-4.80762859173676,-30.0003272062035,
-80.0364283036621));
#29555=CARTESIAN_POINT('Ctrl Pts',(-4.81562085393833,-30.0004142810683,
-80.0407056831963));
#29556=CARTESIAN_POINT('Ctrl Pts',(-4.8242508272187,-30.000508303729,-80.0453243593808));
#29557=CARTESIAN_POINT('Ctrl Pts',(-4.83362976955803,-30.0006265572524,
-80.0503457549901));
#29558=CARTESIAN_POINT('Ctrl Pts',(-4.84365690035937,-30.0007762101847,
-80.0557156911153));
#29559=CARTESIAN_POINT('Ctrl Pts',(-4.85499010112282,-30.0009453559513,
-80.0617850807941));
#29560=CARTESIAN_POINT('Ctrl Pts',(-4.86715064877518,-30.0011547962203,
-80.0682993507869));
#29561=CARTESIAN_POINT('Ctrl Pts',(-4.87993057163511,-30.0014122484325,
-80.0751465187787));
#29562=CARTESIAN_POINT('Ctrl Pts',(-4.89907991110256,-30.0017980128745,
-80.0854062633565));
#29563=CARTESIAN_POINT('Ctrl Pts',(-4.91961655620725,-30.0022930469157,
-80.0964116614511));
#29564=CARTESIAN_POINT('Ctrl Pts',(-4.94072156757471,-30.0029030737397,
-80.1077212473092));
#29565=CARTESIAN_POINT('Ctrl Pts',(-4.95561362249427,-30.0033335190405,
-80.1157014834145));
#29566=CARTESIAN_POINT('Ctrl Pts',(-4.97078474057349,-30.003820567599,-80.1238310489004));
#29567=CARTESIAN_POINT('Ctrl Pts',(-4.98596678089125,-30.0043584577033,
-80.1319652782344));
#29568=CARTESIAN_POINT('Ctrl Pts',(-4.99882878382487,-30.0048141503476,
-80.1388564785847));
#29569=CARTESIAN_POINT('Ctrl Pts',(-5.01169802485068,-30.0053061295215,
-80.1457507055734));
#29570=CARTESIAN_POINT('Ctrl Pts',(-5.02444777245903,-30.0058286173219,
-80.1525794760373));
#29571=CARTESIAN_POINT('Ctrl Pts',(-5.03614342853803,-30.0063079081916,
-80.1588436746115));
#29572=CARTESIAN_POINT('Ctrl Pts',(-5.04773815869922,-30.0068127545887,
-80.1650525968365));
#29573=CARTESIAN_POINT('Ctrl Pts',(-5.05917370952967,-30.0073386464146,
-80.1711745598128));
#29574=CARTESIAN_POINT('Ctrl Pts',(-5.06994987742711,-30.0078342149006,
-80.1769435255471));
#29575=CARTESIAN_POINT('Ctrl Pts',(-5.08058442371394,-30.0083483842256,
-80.1826351325825));
#29576=CARTESIAN_POINT('Ctrl Pts',(-5.09106981935722,-30.0088787394278,
-80.1882448556992));
#29577=CARTESIAN_POINT('Ctrl Pts',(-5.10108922385955,-30.0093855246251,
-80.1936052719358));
#29578=CARTESIAN_POINT('Ctrl Pts',(-5.11097222934838,-30.0099070182464,
-80.1988908141908));
#29579=CARTESIAN_POINT('Ctrl Pts',(-5.12075449580623,-30.0104435082543,
-80.2041199797976));
#29580=CARTESIAN_POINT('Ctrl Pts',(-5.13066213607484,-30.0109868741531,
-80.2094161646808));
#29581=CARTESIAN_POINT('Ctrl Pts',(-5.14046580534474,-30.0115455183055,
-80.2146541901608));
#29582=CARTESIAN_POINT('Ctrl Pts',(-5.15025372270428,-30.0121235896603,
-80.2198803702353));
#29583=CARTESIAN_POINT('Ctrl Pts',(-5.15964979940463,-30.0126785190276,
-80.2248973301284));
#29584=CARTESIAN_POINT('Ctrl Pts',(-5.16903937197897,-30.0132518166605,
-80.2299076190967));
#29585=CARTESIAN_POINT('Ctrl Pts',(-5.17851048157321,-30.0138491970066,
-80.2349574169266));
#29586=CARTESIAN_POINT('Ctrl Pts',(-5.18857236361835,-30.0144838397081,
-80.2403222022889));
#29587=CARTESIAN_POINT('Ctrl Pts',(-5.1987263082372,-30.0151457246997,-80.2457315928303));
#29588=CARTESIAN_POINT('Ctrl Pts',(-5.20902221469754,-30.0158395174066,
-80.2512114235356));
#29589=CARTESIAN_POINT('Ctrl Pts',(-5.21965634603708,-30.0165561014972,
-80.2568712689959));
#29590=CARTESIAN_POINT('Ctrl Pts',(-5.23044154664282,-30.0173067739427,
-80.2626060532407));
#29591=CARTESIAN_POINT('Ctrl Pts',(-5.24137829908528,-30.0180935545994,
-80.268415427425));
#29592=CARTESIAN_POINT('Ctrl Pts',(-5.25298609557392,-30.0189286095934,
-80.2745812461735));
#29593=CARTESIAN_POINT('Ctrl Pts',(-5.26476428837502,-30.0198044087532,
-80.2808309052075));
#29594=CARTESIAN_POINT('Ctrl Pts',(-5.2766581599697,-30.0207189336069,-80.2871349164031));
#29595=CARTESIAN_POINT('Ctrl Pts',(-5.28959276745022,-30.0217134810862,
-80.2939905403031));
#29596=CARTESIAN_POINT('Ctrl Pts',(-5.30266369650548,-30.0227539199694,
-80.3009101655443));
#29597=CARTESIAN_POINT('Ctrl Pts',(-5.31574313110297,-30.0238311868593,
-80.3078259605203));
#29598=CARTESIAN_POINT('Ctrl Pts',(-5.33103182386516,-30.0250904157947,
-80.3159099081716));
#29599=CARTESIAN_POINT('Ctrl Pts',(-5.34633124270374,-30.0264001451606,
-80.3239880989655));
#29600=CARTESIAN_POINT('Ctrl Pts',(-5.36137151862682,-30.0277348059174,
-80.331918671078));
#29601=CARTESIAN_POINT('Ctrl Pts',(-5.3804794850386,-30.0294304299233,-80.3419940916572));
#29602=CARTESIAN_POINT('Ctrl Pts',(-5.39916371312678,-30.0311663675709,
-80.3518282328887));
#29603=CARTESIAN_POINT('Ctrl Pts',(-5.41681836687482,-30.032869487213,-80.3611060033595));
#29604=CARTESIAN_POINT('Ctrl Pts',(-5.42939363939264,-30.0340826060843,
-80.3677144870881));
#29605=CARTESIAN_POINT('Ctrl Pts',(-5.44144478107398,-30.0352784415749,
-80.3740398610588));
#29606=CARTESIAN_POINT('Ctrl Pts',(-5.45277520515776,-30.0364281559369,
-80.3799810695321));
#29607=CARTESIAN_POINT('Ctrl Pts',(-5.46295272876472,-30.0374608838361,
-80.3853177444037));
#29608=CARTESIAN_POINT('Ctrl Pts',(-5.47254808492725,-30.0384562049433,
-80.3903441398836));
#29609=CARTESIAN_POINT('Ctrl Pts',(-5.48145278810254,-30.0393952767108,
-80.3950052139099));
#29610=CARTESIAN_POINT('Ctrl Pts',(-5.48976990866469,-30.0402723832188,
-80.3993587239443));
#29611=CARTESIAN_POINT('Ctrl Pts',(-5.49748410046507,-30.0411003010874,
-80.4033933349473));
#29612=CARTESIAN_POINT('Ctrl Pts',(-5.50454551684857,-30.0418676601101,
-80.4070844377734));
#29613=CARTESIAN_POINT('Ctrl Pts',(-5.51126001057488,-30.042597319298,-80.4105941991899));
#29614=CARTESIAN_POINT('Ctrl Pts',(-5.51738399137094,-30.0432721483508,
-80.413793229439));
#29615=CARTESIAN_POINT('Ctrl Pts',(-5.52291574173486,-30.0438874474019,
-80.4166817509419));
#29616=CARTESIAN_POINT('Ctrl Pts',(-5.5284930595309,-30.0445078149387,-80.419594066452));
#29617=CARTESIAN_POINT('Ctrl Pts',(-5.53346765422382,-30.0450675579802,
-80.422190383135));
#29618=CARTESIAN_POINT('Ctrl Pts',(-5.53788859927536,-30.0455685938731,
-80.4244972069931));
#29619=CARTESIAN_POINT('Ctrl Pts',(-5.5419030547062,-30.0460235613604,-80.4265919268906));
#29620=CARTESIAN_POINT('Ctrl Pts',(-5.54546126449629,-30.0464301580792,
-80.4284480840646));
#29621=CARTESIAN_POINT('Ctrl Pts',(-5.54864302299335,-30.0467956231858,
-80.4301077334735));
#29622=CARTESIAN_POINT('Ctrl Pts',(-5.55175296235284,-30.0471528389582,
-80.4317299210232));
#29623=CARTESIAN_POINT('Ctrl Pts',(-5.55450305873677,-30.0474707401459,
-80.4331642707516));
#29624=CARTESIAN_POINT('Ctrl Pts',(-5.55701120543205,-30.047761872528,-80.4344724313979));
#29625=CARTESIAN_POINT('Ctrl Pts',(-5.5594471567617,-30.0480446248546,-80.4357429374937));
#29626=CARTESIAN_POINT('Ctrl Pts',(-5.56165478585712,-30.0483021202198,
-80.4368943615289));
#29627=CARTESIAN_POINT('Ctrl Pts',(-5.56378554069762,-30.0485515407009,
-80.4380056057852));
#29628=CARTESIAN_POINT('Ctrl Pts',(-5.56463185204192,-30.0486506076507,
-80.4384469792378));
#29629=CARTESIAN_POINT('Ctrl Pts',(-5.56546653509834,-30.0487484655939,
-80.4388822717834));
#29630=CARTESIAN_POINT('Ctrl Pts',(-5.56630111765683,-30.048846456053,-80.4393174796692));
#29631=CARTESIAN_POINT('',(-6.03657504381102,-30.0039988387189,-79.5595261020443));
#29632=CARTESIAN_POINT('Ctrl Pts',(-6.03657504381102,-30.0039988387189,
-79.5595261020443));
#29633=CARTESIAN_POINT('Ctrl Pts',(-5.87981706842629,-30.018948044497,-79.8527898945859));
#29634=CARTESIAN_POINT('Ctrl Pts',(-5.72305909304156,-30.033897250275,-80.1460536871276));
#29635=CARTESIAN_POINT('Ctrl Pts',(-5.56630111765684,-30.048846456053,-80.4393174796692));
#29636=CARTESIAN_POINT('',(-5.8,-30.,-79.4330532904862));
#29637=CARTESIAN_POINT('Ctrl Pts',(-6.03657504381102,-30.0039988387189,
-79.5595261020443));
#29638=CARTESIAN_POINT('Ctrl Pts',(-6.03574564719913,-30.0039707920484,
-79.5590825174968));
#29639=CARTESIAN_POINT('Ctrl Pts',(-6.03491215932269,-30.0039427389739,
-79.5586367469676));
#29640=CARTESIAN_POINT('Ctrl Pts',(-6.03395240733885,-30.0039106444314,
-79.5581234464649));
#29641=CARTESIAN_POINT('Ctrl Pts',(-6.03295612114493,-30.0038773281683,
-79.5575906065097));
#29642=CARTESIAN_POINT('Ctrl Pts',(-6.03182396197816,-30.0038396613357,
-79.5569850974549));
#29643=CARTESIAN_POINT('Ctrl Pts',(-6.03047057385369,-30.0037950777162,
-79.5562612724383));
#29644=CARTESIAN_POINT('Ctrl Pts',(-6.02905379370678,-30.0037484058224,
-79.5555035438202));
#29645=CARTESIAN_POINT('Ctrl Pts',(-6.02739480822809,-30.0036941607515,
-79.5546162808493));
#29646=CARTESIAN_POINT('Ctrl Pts',(-6.02544771415954,-30.0036314185014,
-79.5535749449113));
#29647=CARTESIAN_POINT('Ctrl Pts',(-6.02338219594345,-30.003564860207,-79.5524702739127));
#29648=CARTESIAN_POINT('Ctrl Pts',(-6.02099276816558,-30.0034887568951,
-79.5511923847346));
#29649=CARTESIAN_POINT('Ctrl Pts',(-6.01827775435437,-30.0034040546882,
-79.5497404011225));
#29650=CARTESIAN_POINT('Ctrl Pts',(-6.01532769210741,-30.0033120195088,
-79.5481627141069));
#29651=CARTESIAN_POINT('Ctrl Pts',(-6.01199369456653,-30.0032098704196,
-79.5463797332273));
#29652=CARTESIAN_POINT('Ctrl Pts',(-6.00832872223355,-30.0031007479389,
-79.5444198111003));
#29653=CARTESIAN_POINT('Ctrl Pts',(-6.00402471448509,-30.0029725985398,
-79.5421181511546));
#29654=CARTESIAN_POINT('Ctrl Pts',(-5.99926505507077,-30.0028349230635,
-79.5395728983283));
#29655=CARTESIAN_POINT('Ctrl Pts',(-5.99419984919499,-30.0026943457805,
-79.5368643656081));
#29656=CARTESIAN_POINT('Ctrl Pts',(-5.98739362888286,-30.0025054492218,
-79.5332248550199));
#29657=CARTESIAN_POINT('Ctrl Pts',(-5.98004189473503,-30.0023117546125,
-79.529293835965));
#29658=CARTESIAN_POINT('Ctrl Pts',(-5.9725699777804,-30.0021274945332,-79.5252987934978));
#29659=CARTESIAN_POINT('Ctrl Pts',(-5.96758546735511,-30.0020045747668,
-79.5226337035419));
#29660=CARTESIAN_POINT('Ctrl Pts',(-5.96254896392867,-30.0018857753864,
-79.5199409169067));
#29661=CARTESIAN_POINT('Ctrl Pts',(-5.95756360394063,-30.0017735310499,
-79.5172755775885));
#29662=CARTESIAN_POINT('Ctrl Pts',(-5.95308502270938,-30.0016726967311,
-79.5148811790548));
#29663=CARTESIAN_POINT('Ctrl Pts',(-5.94864830234915,-30.0015771320006,
-79.5125092444795));
#29664=CARTESIAN_POINT('Ctrl Pts',(-5.94429524911591,-30.0014873808014,
-79.5101821179178));
#29665=CARTESIAN_POINT('Ctrl Pts',(-5.94022891457763,-30.0014035411647,
-79.5080082701366));
#29666=CARTESIAN_POINT('Ctrl Pts',(-5.93623596369729,-30.0013247573059,
-79.5058737224368));
#29667=CARTESIAN_POINT('Ctrl Pts',(-5.93231359137331,-30.0012506036051,
-79.5037769652748));
#29668=CARTESIAN_POINT('Ctrl Pts',(-5.92852559777125,-30.0011789903769,
-79.5017520420756));
#29669=CARTESIAN_POINT('Ctrl Pts',(-5.92480383064746,-30.0011116815999,
-79.4997625786459));
#29670=CARTESIAN_POINT('Ctrl Pts',(-5.92110444095789,-30.0010476702309,
-79.4977851219757));
#29671=CARTESIAN_POINT('Ctrl Pts',(-5.91728378123075,-30.0009815604993,
-79.4957428421144));
#29672=CARTESIAN_POINT('Ctrl Pts',(-5.91348056649595,-30.0009188424662,
-79.4937099346464));
#29673=CARTESIAN_POINT('Ctrl Pts',(-5.90962244959741,-30.0008584155952,
-79.4916477111548));
#29674=CARTESIAN_POINT('Ctrl Pts',(-5.90570478328609,-30.0007970560453,
-79.4895536575758));
#29675=CARTESIAN_POINT('Ctrl Pts',(-5.90173064346982,-30.0007380879181,
-79.4874294492513));
#29676=CARTESIAN_POINT('Ctrl Pts',(-5.89767668975181,-30.0006815142988,
-79.4852625989908));
#29677=CARTESIAN_POINT('Ctrl Pts',(-5.89333842135675,-30.0006209730194,
-79.4829437816939));
#29678=CARTESIAN_POINT('Ctrl Pts',(-5.88890914683469,-30.000563210484,-79.4805763431629));
#29679=CARTESIAN_POINT('Ctrl Pts',(-5.88441427394656,-30.0005090020521,
-79.4781738543067));
#29680=CARTESIAN_POINT('Ctrl Pts',(-5.87941082856876,-30.0004486602059,
-79.4754995357972));
#29681=CARTESIAN_POINT('Ctrl Pts',(-5.87432672334003,-30.0003927773851,
-79.4727821196766));
#29682=CARTESIAN_POINT('Ctrl Pts',(-5.86925423225277,-30.0003425904324,
-79.4700709150979));
#29683=CARTESIAN_POINT('Ctrl Pts',(-5.86215627755727,-30.0002723636521,
-79.4662771169545));
#29684=CARTESIAN_POINT('Ctrl Pts',(-5.85508269024457,-30.0002135200039,
-79.4624963505019));
#29685=CARTESIAN_POINT('Ctrl Pts',(-5.84838446975869,-30.0001672203483,
-79.458916194205));
#29686=CARTESIAN_POINT('Ctrl Pts',(-5.84284768581393,-30.0001289488119,
-79.4559568183609));
#29687=CARTESIAN_POINT('Ctrl Pts',(-5.83757231667413,-30.0000991731415,
-79.4531371523948));
#29688=CARTESIAN_POINT('Ctrl Pts',(-5.83274900607812,-30.0000766073763,
-79.450559082205));
#29689=CARTESIAN_POINT('Ctrl Pts',(-5.82874247887498,-30.0000578629163,
-79.4484175845466));
#29690=CARTESIAN_POINT('Ctrl Pts',(-5.82504874387763,-30.0000440365559,
-79.4464432539887));
#29691=CARTESIAN_POINT('Ctrl Pts',(-5.82174274620944,-30.0000337677252,
-79.4446761456858));
#29692=CARTESIAN_POINT('Ctrl Pts',(-5.81868753713252,-30.0000242778744,
-79.4430430878712));
#29693=CARTESIAN_POINT('Ctrl Pts',(-5.81596405942472,-30.0000178010199,
-79.4415873205933));
#29694=CARTESIAN_POINT('Ctrl Pts',(-5.81358977837239,-30.0000131915893,
-79.4403181802751));
#29695=CARTESIAN_POINT('Ctrl Pts',(-5.81143204918921,-30.0000090025726,
-79.4391647948748));
#29696=CARTESIAN_POINT('Ctrl Pts',(-5.80956279681059,-30.0000063473931,
-79.4381655849932));
#29697=CARTESIAN_POINT('Ctrl Pts',(-5.80795543373066,-30.000004520639,-79.4373063426729));
#29698=CARTESIAN_POINT('Ctrl Pts',(-5.80640524598471,-30.0000027588642,
-79.436477664366));
#29699=CARTESIAN_POINT('Ctrl Pts',(-5.80509895162393,-30.0000017661867,
-79.4357793357));
#29700=CARTESIAN_POINT('Ctrl Pts',(-5.8039708127979,-30.0000011262397,-79.4351762238893));
#29701=CARTESIAN_POINT('Ctrl Pts',(-5.80289072093286,-30.0000005135478,
-79.4345987983584));
#29702=CARTESIAN_POINT('Ctrl Pts',(-5.80197407678276,-30.0000002263774,
-79.4341087289835));
#29703=CARTESIAN_POINT('Ctrl Pts',(-5.8011210264025,-30.0000000897643,-79.4336526482453));
#29704=CARTESIAN_POINT('Ctrl Pts',(-5.80073919554487,-30.0000000286154,
-79.4334485035623));
#29705=CARTESIAN_POINT('Ctrl Pts',(-5.80036951503659,-30.,-79.4332508528029));
#29706=CARTESIAN_POINT('Ctrl Pts',(-5.8,-30.,-79.4330532904862));
#29707=CARTESIAN_POINT('',(-5.26966991411008,-30.,-79.7165266452431));
#29708=CARTESIAN_POINT('Ctrl Pts',(-12.7960010943682,-36.7634229774484,
-79.559527160348));
#29709=CARTESIAN_POINT('Ctrl Pts',(-12.796112684693,-36.766722900773,-79.5577622689418));
#29710=CARTESIAN_POINT('Ctrl Pts',(-12.7966304463649,-36.779733004731,-79.5508027625369));
#29711=CARTESIAN_POINT('Ctrl Pts',(-12.798503621254,-36.8493462580203,-79.5135787011833));
#29712=CARTESIAN_POINT('Ctrl Pts',(-12.7995831813545,-36.9140618669959,
-79.4789882204304));
#29713=CARTESIAN_POINT('Ctrl Pts',(-12.800077777097,-36.9836467597157,-79.4417959628394));
#29714=CARTESIAN_POINT('Ctrl Pts',(-12.8,-36.9966978147859,-79.4348188136624));
#29715=CARTESIAN_POINT('Ctrl Pts',(-12.8,-37.,-79.4330532904862));
#29716=CARTESIAN_POINT('Ctrl Pts',(-12.7810518328599,-36.9201809478066,
-79.8527909466985));
#29717=CARTESIAN_POINT('Ctrl Pts',(-12.7813470858521,-36.9262391322969,
-79.8495905651427));
#29718=CARTESIAN_POINT('Ctrl Pts',(-12.7831737363863,-36.9560219574473,
-79.8337980696517));
#29719=CARTESIAN_POINT('Ctrl Pts',(-12.7889123048375,-37.0722811924033,
-79.7718566610738));
#29720=CARTESIAN_POINT('Ctrl Pts',(-12.7951961994244,-37.2013837171206,
-79.7031096229565));
#29721=CARTESIAN_POINT('Ctrl Pts',(-12.7992412708901,-37.3176322921036,
-79.6411502857689));
#29722=CARTESIAN_POINT('Ctrl Pts',(-12.8,-37.3474826193307,-79.6252655486096));
#29723=CARTESIAN_POINT('Ctrl Pts',(-12.8,-37.3535533905933,-79.6220355269908));
#29724=CARTESIAN_POINT('Ctrl Pts',(-12.7661025713516,-37.0769389181648,
-80.146054733049));
#29725=CARTESIAN_POINT('Ctrl Pts',(-12.7668146458603,-37.0857693916081,
-80.1414232484696));
#29726=CARTESIAN_POINT('Ctrl Pts',(-12.771474141461,-37.1146188178936,-80.126276652849));
#29727=CARTESIAN_POINT('Ctrl Pts',(-12.7845596965995,-37.3111973977879,
-80.0204512333998));
#29728=CARTESIAN_POINT('Ctrl Pts',(-12.7958833886632,-37.4728678413485,
-79.9346812492863));
#29729=CARTESIAN_POINT('Ctrl Pts',(-12.7990076133253,-37.6692758524317,
-79.8304581598936));
#29730=CARTESIAN_POINT('Ctrl Pts',(-12.8,-37.6982674238754,-79.8157122835568));
#29731=CARTESIAN_POINT('Ctrl Pts',(-12.8,-37.7071067811866,-79.8110177634954));
#29732=CARTESIAN_POINT('Ctrl Pts',(-12.7511533098433,-37.2336968885229,
-80.4393185193995));
#29733=CARTESIAN_POINT('Ctrl Pts',(-12.7525119116407,-37.2452680428387,
-80.4332845365905));
#29734=CARTESIAN_POINT('Ctrl Pts',(-12.7587851319936,-37.2908525231663,
-80.4097062662184));
#29735=CARTESIAN_POINT('Ctrl Pts',(-12.7815887113731,-37.5340742166441,
-80.281832792717));
#29736=CARTESIAN_POINT('Ctrl Pts',(-12.7948941008387,-37.7601548957666,
-80.1608661463623));
#29737=CARTESIAN_POINT('Ctrl Pts',(-12.8009520655495,-38.0032538535837,
-80.0305401854391));
#29738=CARTESIAN_POINT('Ctrl Pts',(-12.8,-38.0490522284202,-80.006159018504));
#29739=CARTESIAN_POINT('Ctrl Pts',(-12.8,-38.0606601717798,-80.));
#29740=CARTESIAN_POINT('',(-12.8,-37.,-79.4330532904862));
#29741=CARTESIAN_POINT('',(-12.7960010943682,-36.7634229774484,-79.559527160348));
#29742=CARTESIAN_POINT('Ctrl Pts',(-12.8,-37.,-79.4330532904862));
#29743=CARTESIAN_POINT('Ctrl Pts',(-12.8,-36.9991700472799,-79.433497027184));
#29744=CARTESIAN_POINT('Ctrl Pts',(-12.7999998681034,-36.9983360052531,
-79.4339429495663));
#29745=CARTESIAN_POINT('Ctrl Pts',(-12.7999995080477,-36.9973756274263,
-79.4344563936114));
#29746=CARTESIAN_POINT('Ctrl Pts',(-12.7999991342866,-36.9963786928142,
-79.4349893819059));
#29747=CARTESIAN_POINT('Ctrl Pts',(-12.7999985165436,-36.9952458083565,
-79.4355950301756));
#29748=CARTESIAN_POINT('Ctrl Pts',(-12.7999973347952,-36.9938915746925,
-79.4363189798575));
#29749=CARTESIAN_POINT('Ctrl Pts',(-12.7999960976967,-36.9924739120601,
-79.4370768375589));
#29750=CARTESIAN_POINT('Ctrl Pts',(-12.7999942436752,-36.9908139133176,
-79.4379642131993));
#29751=CARTESIAN_POINT('Ctrl Pts',(-12.7999911447529,-36.9888656665758,
-79.4390056428451));
#29752=CARTESIAN_POINT('Ctrl Pts',(-12.7999878573614,-36.9867989320079,
-79.4401104098148));
#29753=CARTESIAN_POINT('Ctrl Pts',(-12.7999831623485,-36.9844081334042,
-79.4413883725713));
#29754=CARTESIAN_POINT('Ctrl Pts',(-12.7999760573464,-36.9816916254731,
-79.4428404082825));
#29755=CARTESIAN_POINT('Ctrl Pts',(-12.7999683372862,-36.9787399578497,
-79.4444181422356));
#29756=CARTESIAN_POINT('Ctrl Pts',(-12.7999577493633,-36.9754042150751,
-79.4462011422145));
#29757=CARTESIAN_POINT('Ctrl Pts',(-12.7999429445767,-36.971737433388,-79.4481610614896));
#29758=CARTESIAN_POINT('Ctrl Pts',(-12.7999255589313,-36.9674314364342,
-79.4504626455894));
#29759=CARTESIAN_POINT('Ctrl Pts',(-12.7999022941935,-36.962669730668,-79.4530077769879));
#29760=CARTESIAN_POINT('Ctrl Pts',(-12.7998716028383,-36.957602549858,-79.4557161648616));
#29761=CARTESIAN_POINT('Ctrl Pts',(-12.7998303537853,-36.9507922800498,
-79.4593562268323));
#29762=CARTESIAN_POINT('Ctrl Pts',(-12.7997754571375,-36.9434364114665,
-79.4632878755981));
#29763=CARTESIAN_POINT('Ctrl Pts',(-12.7997070636587,-36.9359607700949,
-79.4672835422778));
#29764=CARTESIAN_POINT('Ctrl Pts',(-12.7996614454932,-36.9309745484407,
-79.4699486353087));
#29765=CARTESIAN_POINT('Ctrl Pts',(-12.7996099514239,-36.9259365295086,
-79.4726414139089));
#29766=CARTESIAN_POINT('Ctrl Pts',(-12.799553634361,-36.9209498911825,-79.4753067403585));
#29767=CARTESIAN_POINT('Ctrl Pts',(-12.7995030421141,-36.9164701611609,
-79.4777011275455));
#29768=CARTESIAN_POINT('Ctrl Pts',(-12.7994485979144,-36.9120324824234,
-79.4800730469208));
#29769=CARTESIAN_POINT('Ctrl Pts',(-12.7993911715046,-36.9076786684244,
-79.4824001575494));
#29770=CARTESIAN_POINT('Ctrl Pts',(-12.7993375275474,-36.9036116231,-79.4845739905159));
#29771=CARTESIAN_POINT('Ctrl Pts',(-12.7992813111153,-36.8996181331004,
-79.4867085227894));
#29772=CARTESIAN_POINT('Ctrl Pts',(-12.7992228531719,-36.8956953901507,
-79.4888052645999));
#29773=CARTESIAN_POINT('Ctrl Pts',(-12.7991663978579,-36.8919070309902,
-79.4908301770519));
#29774=CARTESIAN_POINT('Ctrl Pts',(-12.7991078794155,-36.888185055055,-79.492819629682));
#29775=CARTESIAN_POINT('Ctrl Pts',(-12.7990468226819,-36.8844856116882,
-79.4947970740634));
#29776=CARTESIAN_POINT('Ctrl Pts',(-12.7989837615226,-36.8806647196525,
-79.4968394357754));
#29777=CARTESIAN_POINT('Ctrl Pts',(-12.7989179009539,-36.8768614401243,
-79.4988724221631));
#29778=CARTESIAN_POINT('Ctrl Pts',(-12.7988478958076,-36.8730034199306,
-79.500934726048));
#29779=CARTESIAN_POINT('Ctrl Pts',(-12.7987768114531,-36.869085924007,-79.5030288226719));
#29780=CARTESIAN_POINT('Ctrl Pts',(-12.7987014293895,-36.8651121239306,
-79.5051530744746));
#29781=CARTESIAN_POINT('Ctrl Pts',(-12.798620957786,-36.861058684193,-79.507319968484));
#29782=CARTESIAN_POINT('Ctrl Pts',(-12.7985348425268,-36.8567209675521,
-79.5096388316748));
#29783=CARTESIAN_POINT('Ctrl Pts',(-12.7984428756104,-36.8522924453854,
-79.5120063163369));
#29784=CARTESIAN_POINT('Ctrl Pts',(-12.7983451408915,-36.8477985251063,
-79.5144088487625));
#29785=CARTESIAN_POINT('Ctrl Pts',(-12.7982363480041,-36.8427961414171,
-79.517083215078));
#29786=CARTESIAN_POINT('Ctrl Pts',(-12.7981203741976,-36.8377133475194,
-79.5198006757509));
#29787=CARTESIAN_POINT('Ctrl Pts',(-12.7979991018748,-36.8326423884013,
-79.5225119154));
#29788=CARTESIAN_POINT('Ctrl Pts',(-12.7978294071761,-36.8255466648324,
-79.5263057158687));
#29789=CARTESIAN_POINT('Ctrl Pts',(-12.797649162788,-36.8184757467536,-79.5300864660878));
#29790=CARTESIAN_POINT('Ctrl Pts',(-12.7974690699909,-36.8117804087757,
-79.5336665753703));
#29791=CARTESIAN_POINT('Ctrl Pts',(-12.797320200581,-36.8062458675276,-79.5366259872121));
#29792=CARTESIAN_POINT('Ctrl Pts',(-12.7971716766398,-36.8009728944587,
-79.5394456609008));
#29793=CARTESIAN_POINT('Ctrl Pts',(-12.7970312260022,-36.7961519626054,
-79.5420236982032));
#29794=CARTESIAN_POINT('Ctrl Pts',(-12.7969145602557,-36.7921474409935,
-79.5441651526787));
#29795=CARTESIAN_POINT('Ctrl Pts',(-12.7968035511635,-36.7884556925945,
-79.5461394144843));
#29796=CARTESIAN_POINT('Ctrl Pts',(-12.7967020909069,-36.7851515624929,
-79.5479064262232));
#29797=CARTESIAN_POINT('Ctrl Pts',(-12.7966083305111,-36.78209818419,-79.5495393387112));
#29798=CARTESIAN_POINT('Ctrl Pts',(-12.7965227697646,-36.7793764113463,
-79.5509949492069));
#29799=CARTESIAN_POINT('Ctrl Pts',(-12.7964471432921,-36.7770036522266,
-79.5522639237828));
#29800=CARTESIAN_POINT('Ctrl Pts',(-12.7963784121474,-36.7748472320619,
-79.5534171981886));
#29801=CARTESIAN_POINT('Ctrl Pts',(-12.7963178972973,-36.7729791573364,
-79.5544162789617));
#29802=CARTESIAN_POINT('Ctrl Pts',(-12.7962654049679,-36.7713728291545,
-79.5552753781006));
#29803=CARTESIAN_POINT('Ctrl Pts',(-12.7962147798707,-36.7698236405127,
-79.5561039177746));
#29804=CARTESIAN_POINT('Ctrl Pts',(-12.7961716284115,-36.7685182119286,
-79.5568020948707));
#29805=CARTESIAN_POINT('Ctrl Pts',(-12.7961341448816,-36.7673908281644,
-79.5574050490616));
#29806=CARTESIAN_POINT('Ctrl Pts',(-12.7960982577448,-36.7663114587615,
-79.5579823239218));
#29807=CARTESIAN_POINT('Ctrl Pts',(-12.7960675687105,-36.7653954357194,
-79.5584722369981));
#29808=CARTESIAN_POINT('Ctrl Pts',(-12.7960388778786,-36.7645429567618,
-79.5589281651919));
#29809=CARTESIAN_POINT('Ctrl Pts',(-12.7960260391719,-36.7641614855156,
-79.5591321860592));
#29810=CARTESIAN_POINT('Ctrl Pts',(-12.7960135782664,-36.7637921484035,
-79.5593297173829));
#29811=CARTESIAN_POINT('Ctrl Pts',(-12.7960010943682,-36.7634229774484,
-79.559527160348));
#29812=CARTESIAN_POINT('',(-12.7511533098433,-37.2336968885229,-80.4393185193995));
#29813=CARTESIAN_POINT('Ctrl Pts',(-12.7511533098433,-37.2336968885229,
-80.4393185193995));
#29814=CARTESIAN_POINT('Ctrl Pts',(-12.7661025713516,-37.0769389181648,
-80.146054733049));
#29815=CARTESIAN_POINT('Ctrl Pts',(-12.7810518328599,-36.9201809478066,
-79.8527909466985));
#29816=CARTESIAN_POINT('Ctrl Pts',(-12.7960010943682,-36.7634229774484,
-79.559527160348));
#29817=CARTESIAN_POINT('',(-12.8,-38.0606601717798,-80.));
#29818=CARTESIAN_POINT('Ctrl Pts',(-12.7511533098433,-37.2336968885229,
-80.4393185193995));
#29819=CARTESIAN_POINT('Ctrl Pts',(-12.7513994405692,-37.2357931735541,
-80.4382253745416));
#29820=CARTESIAN_POINT('Ctrl Pts',(-12.7516451610574,-37.2378933689947,
-80.4371300040475));
#29821=CARTESIAN_POINT('Ctrl Pts',(-12.7519098980542,-37.2401660578997,
-80.4359446637797));
#29822=CARTESIAN_POINT('Ctrl Pts',(-12.7521813734055,-37.2424965935867,
-80.4347291530298));
#29823=CARTESIAN_POINT('Ctrl Pts',(-12.7524728330613,-37.2450083893932,
-80.4334190997504));
#29824=CARTESIAN_POINT('Ctrl Pts',(-12.7527989349955,-37.24783495635,-80.4319448106882));
#29825=CARTESIAN_POINT('Ctrl Pts',(-12.7531345289436,-37.2507437976206,
-80.4304276087488));
#29826=CARTESIAN_POINT('Ctrl Pts',(-12.7535068003015,-37.2539858554197,
-80.42873654726));
#29827=CARTESIAN_POINT('Ctrl Pts',(-12.7539253120768,-37.2576582073246,
-80.426820658855));
#29828=CARTESIAN_POINT('Ctrl Pts',(-12.7543667487184,-37.2615317200594,
-80.4247998236171));
#29829=CARTESIAN_POINT('Ctrl Pts',(-12.7548596320871,-37.2658839386598,
-80.4225288661114));
#29830=CARTESIAN_POINT('Ctrl Pts',(-12.755408172194,-37.2707766668765,-80.4199748565295));
#29831=CARTESIAN_POINT('Ctrl Pts',(-12.7559812991956,-37.275888699009,-80.4173063700591));
#29832=CARTESIAN_POINT('Ctrl Pts',(-12.7566151458086,-37.2815905684644,
-80.4143289939935));
#29833=CARTESIAN_POINT('Ctrl Pts',(-12.7573073447791,-37.2878992679656,
-80.411032794402));
#29834=CARTESIAN_POINT('Ctrl Pts',(-12.7580393314685,-37.2945705926274,
-80.4075471286764));
#29835=CARTESIAN_POINT('Ctrl Pts',(-12.7588364999907,-37.30192023826,-80.4037050658652));
#29836=CARTESIAN_POINT('Ctrl Pts',(-12.7596890377365,-37.3099134194748,
-80.3995233101776));
#29837=CARTESIAN_POINT('Ctrl Pts',(-12.7606097179899,-37.3185454878402,
-80.395007310851));
#29838=CARTESIAN_POINT('Ctrl Pts',(-12.7615948440084,-37.3279276832095,
-80.3900953298116));
#29839=CARTESIAN_POINT('Ctrl Pts',(-12.7626256502735,-37.3379589184685,
-80.3848383516342));
#29840=CARTESIAN_POINT('Ctrl Pts',(-12.7637911119095,-37.3493005451655,
-80.3788946485406));
#29841=CARTESIAN_POINT('Ctrl Pts',(-12.7650147097049,-37.3614711578117,
-80.3725102492067));
#29842=CARTESIAN_POINT('Ctrl Pts',(-12.7662645085333,-37.3742620271656,
-80.3657921301537));
#29843=CARTESIAN_POINT('Ctrl Pts',(-12.7681310603188,-37.3933649575649,
-80.3557587417162));
#29844=CARTESIAN_POINT('Ctrl Pts',(-12.7700542611625,-37.4138480222161,
-80.3449824308113));
#29845=CARTESIAN_POINT('Ctrl Pts',(-12.771933161456,-37.4348978198511,-80.3338856192622));
#29846=CARTESIAN_POINT('Ctrl Pts',(-12.7732621154593,-37.4497864293912,
-80.3260367982351));
#29847=CARTESIAN_POINT('Ctrl Pts',(-12.7745690686291,-37.4649546500062,
-80.3180298208842));
#29848=CARTESIAN_POINT('Ctrl Pts',(-12.7758280668251,-37.4801342690844,
-80.3100055650248));
#29849=CARTESIAN_POINT('Ctrl Pts',(-12.7768947488483,-37.4929951507302,
-80.3032070410057));
#29850=CARTESIAN_POINT('Ctrl Pts',(-12.7779271339726,-37.5058636123494,
-80.2963964675831));
#29851=CARTESIAN_POINT('Ctrl Pts',(-12.7789158806655,-37.518612876001,-80.2896410489724));
#29852=CARTESIAN_POINT('Ctrl Pts',(-12.7798229044688,-37.5303083746442,
-80.2834439860397));
#29853=CARTESIAN_POINT('Ctrl Pts',(-12.780693275662,-37.5419031904326,-80.2772935520739));
#29854=CARTESIAN_POINT('Ctrl Pts',(-12.7815244506041,-37.5533390685944,
-80.2712210383768));
#29855=CARTESIAN_POINT('Ctrl Pts',(-12.7823077096733,-37.5641156871265,
-80.2654985951398));
#29856=CARTESIAN_POINT('Ctrl Pts',(-12.7830562158113,-37.574750894505,-80.2598455004758));
#29857=CARTESIAN_POINT('Ctrl Pts',(-12.7837713234296,-37.5852372054239,
-80.2542662705478));
#29858=CARTESIAN_POINT('Ctrl Pts',(-12.7844546559708,-37.5952575678206,
-80.2489349480068));
#29859=CARTESIAN_POINT('Ctrl Pts',(-12.7851075373859,-37.6051417606873,
-80.2436711904462));
#29860=CARTESIAN_POINT('Ctrl Pts',(-12.785733730508,-37.6149255321358,-80.2384566030175));
#29861=CARTESIAN_POINT('Ctrl Pts',(-12.7863647839694,-37.6247852425343,
-80.2332015413918));
#29862=CARTESIAN_POINT('Ctrl Pts',(-12.7869687646608,-37.6345423851848,
-80.2279967299011));
#29863=CARTESIAN_POINT('Ctrl Pts',(-12.7875516726604,-37.6442838772853,
-80.2227966528135));
#29864=CARTESIAN_POINT('Ctrl Pts',(-12.7881141164258,-37.6536833734367,
-80.2177791355722));
#29865=CARTESIAN_POINT('Ctrl Pts',(-12.7886574186774,-37.6630762514784,
-80.2127618146277));
#29866=CARTESIAN_POINT('Ctrl Pts',(-12.7891861182228,-37.6725507961374,
-80.2076983078163));
#29867=CARTESIAN_POINT('Ctrl Pts',(-12.7897476952908,-37.6826145214739,
-80.2023199235641));
#29868=CARTESIAN_POINT('Ctrl Pts',(-12.7902927397347,-37.692770424443,-80.1968894029537));
#29869=CARTESIAN_POINT('Ctrl Pts',(-12.7908223045103,-37.7030685797929,
-80.1913806465253));
#29870=CARTESIAN_POINT('Ctrl Pts',(-12.791368938445,-37.7136986697069,-80.1856943294948));
#29871=CARTESIAN_POINT('Ctrl Pts',(-12.7918989840159,-37.7244799526093,
-80.1799248452));
#29872=CARTESIAN_POINT('Ctrl Pts',(-12.7924102981559,-37.735413051101,-80.1740724096529));
#29873=CARTESIAN_POINT('Ctrl Pts',(-12.792952958374,-37.7470164024437,-80.1678611909471));
#29874=CARTESIAN_POINT('Ctrl Pts',(-12.793474411486,-37.7587904314581,-80.1615567035672));
#29875=CARTESIAN_POINT('Ctrl Pts',(-12.7939700304283,-37.770680649105,-80.1551886521419));
#29876=CARTESIAN_POINT('Ctrl Pts',(-12.7945089628702,-37.7836099855033,
-80.1482640792262));
#29877=CARTESIAN_POINT('Ctrl Pts',(-12.7950171958874,-37.7966762206018,
-80.141264600033));
#29878=CARTESIAN_POINT('Ctrl Pts',(-12.7954885347944,-37.8097519144859,
-80.1342591058519));
#29879=CARTESIAN_POINT('Ctrl Pts',(-12.7960391658972,-37.8250273004919,
-80.1260750944542));
#29880=CARTESIAN_POINT('Ctrl Pts',(-12.7965391522779,-37.8403147035479,
-80.1178833489533));
#29881=CARTESIAN_POINT('Ctrl Pts',(-12.7969821268525,-37.8553453477091,
-80.1098288897853));
#29882=CARTESIAN_POINT('Ctrl Pts',(-12.7975461188403,-37.8744822538933,
-80.0995740112976));
#29883=CARTESIAN_POINT('Ctrl Pts',(-12.7980169429444,-37.8931974999971,
-80.0895446215398));
#29884=CARTESIAN_POINT('Ctrl Pts',(-12.7983966214117,-37.9108833519335,
-80.0800683678505));
#29885=CARTESIAN_POINT('Ctrl Pts',(-12.7986667701735,-37.9234671864481,
-80.0733258253554));
#29886=CARTESIAN_POINT('Ctrl Pts',(-12.7988912189896,-37.9355281057759,
-80.0668642654862));
#29887=CARTESIAN_POINT('Ctrl Pts',(-12.7990759418347,-37.9468694211329,
-80.0607896272218));
#29888=CARTESIAN_POINT('Ctrl Pts',(-12.7992418553829,-37.9570559136128,
-80.0553335354853));
#29889=CARTESIAN_POINT('Ctrl Pts',(-12.7993758428282,-37.9666612296763,
-80.0501899332581));
#29890=CARTESIAN_POINT('Ctrl Pts',(-12.7994842519168,-37.9755767510305,
-80.0454172471301));
#29891=CARTESIAN_POINT('Ctrl Pts',(-12.7995855041482,-37.9839036952367,
-80.0409596400511));
#29892=CARTESIAN_POINT('Ctrl Pts',(-12.7996645158678,-37.9916285000599,
-80.0368258127267));
#29893=CARTESIAN_POINT('Ctrl Pts',(-12.7997270277937,-37.9987011336137,
-80.0330426135706));
#29894=CARTESIAN_POINT('Ctrl Pts',(-12.7997864674487,-38.0054261687645,
-80.0294453471332));
#29895=CARTESIAN_POINT('Ctrl Pts',(-12.799831031352,-38.0115612592219,-80.0261652513481));
#29896=CARTESIAN_POINT('Ctrl Pts',(-12.7998653971875,-38.0171044476453,
-80.0232033000281));
#29897=CARTESIAN_POINT('Ctrl Pts',(-12.7999000951572,-38.0227012091317,
-80.0202127224387));
#29898=CARTESIAN_POINT('Ctrl Pts',(-12.7999244270517,-38.0276938621132,
-80.0175468476837));
#29899=CARTESIAN_POINT('Ctrl Pts',(-12.7999423966669,-38.0321313874579,
-80.0151792626433));
#29900=CARTESIAN_POINT('Ctrl Pts',(-12.7999586895953,-38.0361548616677,
-80.013032589304));
#29901=CARTESIAN_POINT('Ctrl Pts',(-12.7999697470036,-38.0397222527165,
-80.0111309840731));
#29902=CARTESIAN_POINT('Ctrl Pts',(-12.7999777607813,-38.0429130718287,
-80.0094316690052));
#29903=CARTESIAN_POINT('Ctrl Pts',(-12.799985593692,-38.0460318757299,-80.0077707066388));
#29904=CARTESIAN_POINT('Ctrl Pts',(-12.79999051485,-38.0487907196809,-80.006303109571));
#29905=CARTESIAN_POINT('Ctrl Pts',(-12.7999938354508,-38.0513071548013,
-80.0049656981994));
#29906=CARTESIAN_POINT('Ctrl Pts',(-12.7999970603764,-38.0537510847359,
-80.003666821205));
#29907=CARTESIAN_POINT('Ctrl Pts',(-12.7999987706598,-38.0559662730045,
-80.0024907892758));
#29908=CARTESIAN_POINT('Ctrl Pts',(-12.7999995399946,-38.0581037631129,
-80.0013564738542));
#29909=CARTESIAN_POINT('Ctrl Pts',(-12.7999998496093,-38.0589639847485,
-80.0008999745874));
#29910=CARTESIAN_POINT('Ctrl Pts',(-12.8,-38.059812131143,-80.0004499589473));
#29911=CARTESIAN_POINT('Ctrl Pts',(-12.8,-38.0606601717798,-80.));
#29912=CARTESIAN_POINT('',(-12.8,-37.5303300858899,-79.7165266452431));
#29913=CARTESIAN_POINT('Ctrl Pts',(-12.7511533098433,-37.2336968885229,
-80.4393185193995));
#29914=CARTESIAN_POINT('Ctrl Pts',(-12.6502151549565,-36.3740108725136,
-80.8876169778077));
#29915=CARTESIAN_POINT('Ctrl Pts',(-12.1730890667104,-34.7673104933084,
-81.6648966847297));
#29916=CARTESIAN_POINT('Ctrl Pts',(-11.2444873881411,-33.3688875479671,
-82.0000000010328));
#29917=CARTESIAN_POINT('Ctrl Pts',(-10.7999999953529,-32.8445654686786,
-82.));
#29918=CARTESIAN_POINT('Ctrl Pts',(-12.7661025713516,-37.0769389181648,
-80.146054733049));
#29919=CARTESIAN_POINT('Ctrl Pts',(-12.6891256583696,-36.2174179501799,
-80.5980934851221));
#29920=CARTESIAN_POINT('Ctrl Pts',(-12.254521024505,-34.617670241717,-81.4026172457878));
#29921=CARTESIAN_POINT('Ctrl Pts',(-11.3507989284016,-33.237189874179,-81.7954256760992));
#29922=CARTESIAN_POINT('Ctrl Pts',(-10.9136110332455,-32.7213815205079,
-81.8224303038976));
#29923=CARTESIAN_POINT('Ctrl Pts',(-12.7810518328599,-36.9201809478066,
-79.8527909466985));
#29924=CARTESIAN_POINT('Ctrl Pts',(-12.7280361617827,-36.0608250278462,
-80.3085699924365));
#29925=CARTESIAN_POINT('Ctrl Pts',(-12.3359529822995,-34.4680299901255,
-81.1403378068459));
#29926=CARTESIAN_POINT('Ctrl Pts',(-11.4571104686622,-33.105492200391,-81.5908513511656));
#29927=CARTESIAN_POINT('Ctrl Pts',(-11.0272220711382,-32.5981975723372,
-81.6448606077953));
#29928=CARTESIAN_POINT('Ctrl Pts',(-12.7960010943682,-36.7634229774484,
-79.559527160348));
#29929=CARTESIAN_POINT('Ctrl Pts',(-12.7669466651958,-35.9042321055125,
-80.0190464997509));
#29930=CARTESIAN_POINT('Ctrl Pts',(-12.4173849400941,-34.3183897385341,
-80.878058367904));
#29931=CARTESIAN_POINT('Ctrl Pts',(-11.5634220089227,-32.973794526603,-81.386277026232));
#29932=CARTESIAN_POINT('Ctrl Pts',(-11.1408331090309,-32.4750136241665,
-81.467290911693));
#29933=CARTESIAN_POINT('',(-11.1408331090314,-32.4750136241671,-81.4672909116929));
#29934=CARTESIAN_POINT('Ctrl Pts',(-12.7960010943682,-36.7634229774484,
-79.559527160348));
#29935=CARTESIAN_POINT('Ctrl Pts',(-12.7669466651958,-35.9042321055125,
-80.0190464997509));
#29936=CARTESIAN_POINT('Ctrl Pts',(-12.4173849400941,-34.3183897385341,
-80.878058367904));
#29937=CARTESIAN_POINT('Ctrl Pts',(-11.5634220089227,-32.973794526603,-81.386277026232));
#29938=CARTESIAN_POINT('Ctrl Pts',(-11.1408331090309,-32.4750136241665,
-81.467290911693));
#29939=CARTESIAN_POINT('',(-10.7999999970626,-32.8445654672303,-82.));
#29940=CARTESIAN_POINT('',(-11.1408331090314,-32.4750136241671,-81.4672909116929));
#29941=CARTESIAN_POINT('Ctrl Pts',(-10.7999999953529,-32.8445654686786,
-82.));
#29942=CARTESIAN_POINT('Ctrl Pts',(-11.2444873881411,-33.3688875479671,
-82.0000000010328));
#29943=CARTESIAN_POINT('Ctrl Pts',(-12.1730890667104,-34.7673104933084,
-81.6648966847297));
#29944=CARTESIAN_POINT('Ctrl Pts',(-12.6502151549565,-36.3740108725136,
-80.8876169778077));
#29945=CARTESIAN_POINT('Ctrl Pts',(-12.7511533098433,-37.2336968885229,
-80.4393185193995));
#29946=CARTESIAN_POINT('Origin',(-5.79999999999999,-37.,-81.75));
#29947=CARTESIAN_POINT('',(-10.4428571428571,-32.4509476205455,-82.));
#29948=CARTESIAN_POINT('',(-10.8,-32.1010205144336,-81.5));
#29949=CARTESIAN_POINT('',(-10.4428571428571,-32.4509476205455,-82.));
#29950=CARTESIAN_POINT('',(-10.6989794855664,-32.,-81.5));
#29951=CARTESIAN_POINT('Origin',(-5.79999999999999,-37.,-81.5));
#29952=CARTESIAN_POINT('',(-10.3490523794545,-32.3571428571429,-82.));
#29953=CARTESIAN_POINT('',(-10.6989794855664,-32.,-81.5));
#29954=CARTESIAN_POINT('Origin',(-5.79999999999999,-37.,-82.));
#29955=CARTESIAN_POINT('Ctrl Pts',(-10.7999999953534,-32.8445654686792,
-82.));
#29956=CARTESIAN_POINT('Ctrl Pts',(-10.6842569540723,-32.7080337400726,
-82.));
#29957=CARTESIAN_POINT('Ctrl Pts',(-10.5665688864269,-32.5772103901022,
-82.));
#29958=CARTESIAN_POINT('Ctrl Pts',(-10.4428571428571,-32.4509476205455,
-82.));
#29959=CARTESIAN_POINT('Ctrl Pts',(-10.9136110332461,-32.7213815205085,
-81.8224303038976));
#29960=CARTESIAN_POINT('Ctrl Pts',(-10.7997687569007,-32.5870667377815,
-81.8294622194963));
#29961=CARTESIAN_POINT('Ctrl Pts',(-10.6833507226253,-32.4582555164613,
-81.8333333333333));
#29962=CARTESIAN_POINT('Ctrl Pts',(-10.5619047619048,-32.3343052518416,
-81.8333333333333));
#29963=CARTESIAN_POINT('Ctrl Pts',(-11.0272220711388,-32.5981975723378,
-81.6448606077953));
#29964=CARTESIAN_POINT('Ctrl Pts',(-10.9152805597292,-32.4660997354905,
-81.6589244389925));
#29965=CARTESIAN_POINT('Ctrl Pts',(-10.8001325588236,-32.3393006428204,
-81.6666666666667));
#29966=CARTESIAN_POINT('Ctrl Pts',(-10.6809523809524,-32.2176628831376,
-81.6666666666667));
#29967=CARTESIAN_POINT('Ctrl Pts',(-11.1408331090314,-32.4750136241671,
-81.4672909116929));
#29968=CARTESIAN_POINT('Ctrl Pts',(-11.0307923625576,-32.3451327331994,
-81.4883866584888));
#29969=CARTESIAN_POINT('Ctrl Pts',(-10.916914395022,-32.2203457691795,-81.5));
#29970=CARTESIAN_POINT('Ctrl Pts',(-10.8,-32.1010205144336,-81.5));
#29971=CARTESIAN_POINT('Ctrl Pts',(-10.4428571428571,-32.4509476205455,
-82.));
#29972=CARTESIAN_POINT('Ctrl Pts',(-10.5665688864269,-32.5772103901022,
-82.));
#29973=CARTESIAN_POINT('Ctrl Pts',(-10.6842569540723,-32.7080337400726,
-82.));
#29974=CARTESIAN_POINT('Ctrl Pts',(-10.7999999953534,-32.8445654686792,
-82.));
#29975=CARTESIAN_POINT('Ctrl Pts',(-11.1408331090314,-32.4750136241671,
-81.4672909116929));
#29976=CARTESIAN_POINT('Ctrl Pts',(-11.0307923625576,-32.3451327331994,
-81.4883866584888));
#29977=CARTESIAN_POINT('Ctrl Pts',(-10.916914395022,-32.2203457691795,-81.5));
#29978=CARTESIAN_POINT('Ctrl Pts',(-10.8,-32.1010205144336,-81.5));
#29979=CARTESIAN_POINT('Ctrl Pts',(-9.95543453132142,-32.0000000046471,
-82.));
#29980=CARTESIAN_POINT('Ctrl Pts',(-9.25633811784897,-31.4073498867012,
-82.000000001377));
#29981=CARTESIAN_POINT('Ctrl Pts',(-7.79517610804797,-30.5212430753724,
-81.5542555113626));
#29982=CARTESIAN_POINT('Ctrl Pts',(-6.21107604659501,-30.124551119002,-80.7755468086672));
#29983=CARTESIAN_POINT('Ctrl Pts',(-5.56630111765684,-30.048846456053,-80.4393174796692));
#29984=CARTESIAN_POINT('Ctrl Pts',(-10.0786184794921,-31.8863889667545,
-81.8224303038976));
#29985=CARTESIAN_POINT('Ctrl Pts',(-9.39087370517329,-31.3034715166025,
-81.7864241176491));
#29986=CARTESIAN_POINT('Ctrl Pts',(-7.94673543863312,-30.4455217633812,
-81.2853561028645));
#29987=CARTESIAN_POINT('Ctrl Pts',(-6.36770343773579,-30.0916304595765,
-80.4850846324629));
#29988=CARTESIAN_POINT('Ctrl Pts',(-5.72305909304156,-30.033897250275,-80.1460536871276));
#29989=CARTESIAN_POINT('Ctrl Pts',(-10.2018024276628,-31.7727779288618,
-81.6448606077953));
#29990=CARTESIAN_POINT('Ctrl Pts',(-9.52540929249762,-31.1995931465039,
-81.5728482339212));
#29991=CARTESIAN_POINT('Ctrl Pts',(-8.09829476921827,-30.36980045139,-81.0164566943663));
#29992=CARTESIAN_POINT('Ctrl Pts',(-6.52433082887656,-30.058709800151,-80.1946224562586));
#29993=CARTESIAN_POINT('Ctrl Pts',(-5.87981706842629,-30.018948044497,-79.8527898945859));
#29994=CARTESIAN_POINT('Ctrl Pts',(-10.3249863758336,-31.6591668909691,
-81.467290911693));
#29995=CARTESIAN_POINT('Ctrl Pts',(-9.65994487982194,-31.0957147764052,
-81.3592723501933));
#29996=CARTESIAN_POINT('Ctrl Pts',(-8.24985409980341,-30.2940791393988,
-80.7475572858682));
#29997=CARTESIAN_POINT('Ctrl Pts',(-6.68095822001734,-30.0257891407254,
-79.9041602800544));
#29998=CARTESIAN_POINT('Ctrl Pts',(-6.03657504381102,-30.0039988387189,
-79.5595261020443));
#29999=CARTESIAN_POINT('',(-9.95543453276968,-32.0000000029374,-82.));
#30000=CARTESIAN_POINT('Ctrl Pts',(-5.56630111765684,-30.048846456053,-80.4393174796692));
#30001=CARTESIAN_POINT('Ctrl Pts',(-6.21107604659501,-30.124551119002,-80.7755468086672));
#30002=CARTESIAN_POINT('Ctrl Pts',(-7.79517610804797,-30.5212430753724,
-81.5542555113626));
#30003=CARTESIAN_POINT('Ctrl Pts',(-9.25633811784897,-31.4073498867012,
-82.000000001377));
#30004=CARTESIAN_POINT('Ctrl Pts',(-9.95543453132142,-32.0000000046471,
-82.));
#30005=CARTESIAN_POINT('',(-10.3249863758329,-31.6591668909686,-81.4672909116929));
#30006=CARTESIAN_POINT('',(-9.95543453276968,-32.0000000029374,-82.));
#30007=CARTESIAN_POINT('Ctrl Pts',(-10.3249863758336,-31.6591668909691,
-81.467290911693));
#30008=CARTESIAN_POINT('Ctrl Pts',(-9.65994487982194,-31.0957147764052,
-81.3592723501933));
#30009=CARTESIAN_POINT('Ctrl Pts',(-8.24985409980341,-30.2940791393988,
-80.7475572858682));
#30010=CARTESIAN_POINT('Ctrl Pts',(-6.68095822001734,-30.0257891407254,
-79.9041602800544));
#30011=CARTESIAN_POINT('Ctrl Pts',(-6.03657504381102,-30.0039988387189,
-79.5595261020443));
#30012=CARTESIAN_POINT('Ctrl Pts',(-10.3490523794545,-32.3571428571429,
-82.));
#30013=CARTESIAN_POINT('Ctrl Pts',(-10.2227896098978,-32.2334311135731,
-82.));
#30014=CARTESIAN_POINT('Ctrl Pts',(-10.0919662599274,-32.1157430459277,
-82.));
#30015=CARTESIAN_POINT('Ctrl Pts',(-9.95543453132077,-32.0000000046466,
-82.));
#30016=CARTESIAN_POINT('Ctrl Pts',(-10.4656947481584,-32.2380952380952,
-81.8333333333333));
#30017=CARTESIAN_POINT('Ctrl Pts',(-10.3417444835387,-32.1166492773747,
-81.8333333333333));
#30018=CARTESIAN_POINT('Ctrl Pts',(-10.2129332622185,-32.0002312430993,
-81.8294622194963));
#30019=CARTESIAN_POINT('Ctrl Pts',(-10.0786184794915,-31.8863889667539,
-81.8224303038976));
#30020=CARTESIAN_POINT('Ctrl Pts',(-10.5823371168624,-32.1190476190476,
-81.6666666666667));
#30021=CARTESIAN_POINT('Ctrl Pts',(-10.4606993571796,-31.9998674411764,
-81.6666666666667));
#30022=CARTESIAN_POINT('Ctrl Pts',(-10.3339002645095,-31.8847194402708,
-81.6589244389925));
#30023=CARTESIAN_POINT('Ctrl Pts',(-10.2018024276622,-31.7727779288612,
-81.6448606077953));
#30024=CARTESIAN_POINT('Ctrl Pts',(-10.6989794855664,-32.,-81.5));
#30025=CARTESIAN_POINT('Ctrl Pts',(-10.5796542308205,-31.883085604978,-81.5));
#30026=CARTESIAN_POINT('Ctrl Pts',(-10.4548672668006,-31.7692076374424,
-81.4883866584888));
#30027=CARTESIAN_POINT('Ctrl Pts',(-10.3249863758329,-31.6591668909686,
-81.4672909116929));
#30028=CARTESIAN_POINT('Ctrl Pts',(-9.95543453132077,-32.0000000046466,
-82.));
#30029=CARTESIAN_POINT('Ctrl Pts',(-10.0919662599274,-32.1157430459277,
-82.));
#30030=CARTESIAN_POINT('Ctrl Pts',(-10.2227896098978,-32.2334311135731,
-82.));
#30031=CARTESIAN_POINT('Ctrl Pts',(-10.3490523794545,-32.3571428571429,
-82.));
#30032=CARTESIAN_POINT('Ctrl Pts',(-10.6989794855664,-32.,-81.5));
#30033=CARTESIAN_POINT('Ctrl Pts',(-10.5796542308205,-31.883085604978,-81.5));
#30034=CARTESIAN_POINT('Ctrl Pts',(-10.4548672668006,-31.7692076374424,
-81.4883866584888));
#30035=CARTESIAN_POINT('Ctrl Pts',(-10.3249863758329,-31.6591668909686,
-81.4672909116929));
#30036=CARTESIAN_POINT('Origin',(25.7,-32.,-80.));
#30037=CARTESIAN_POINT('',(35.1393398282202,-30.,-80.));
#30038=CARTESIAN_POINT('',(25.7,-30.,-80.));
#30039=CARTESIAN_POINT('',(35.9663031078275,-30.0488466897261,-80.4393185174872));
#30040=CARTESIAN_POINT('Ctrl Pts',(35.9663031078275,-30.0488466897261,-80.4393185174872));
#30041=CARTESIAN_POINT('Ctrl Pts',(35.9642068228121,-30.0486005589982,-80.4382253726154));
#30042=CARTESIAN_POINT('Ctrl Pts',(35.9621066273875,-30.048354838508,-80.437130002107));
#30043=CARTESIAN_POINT('Ctrl Pts',(35.9598339385104,-30.0480901015045,-80.4359446618037));
#30044=CARTESIAN_POINT('Ctrl Pts',(35.957503402852,-30.0478186261464,-80.4347291510173));
#30045=CARTESIAN_POINT('Ctrl Pts',(35.9549916070864,-30.0475271664789,-80.4334190976791));
#30046=CARTESIAN_POINT('Ctrl Pts',(35.9521650401915,-30.0472010645251,-80.4319448085208));
#30047=CARTESIAN_POINT('Ctrl Pts',(35.9492561989846,-30.0468654705568,-80.4304276064823));
#30048=CARTESIAN_POINT('Ctrl Pts',(35.9460141412712,-30.0464931991705,-80.4287365448548));
#30049=CARTESIAN_POINT('Ctrl Pts',(35.9423417894798,-30.0460746873567,-80.426820656262));
#30050=CARTESIAN_POINT('Ctrl Pts',(35.9384682768646,-30.0456332506747,-80.424799820826));
#30051=CARTESIAN_POINT('Ctrl Pts',(35.9341160584144,-30.0451403672545,-80.4225288630673));
#30052=CARTESIAN_POINT('Ctrl Pts',(35.929223330381,-30.0445918270853,-80.419974853174));
#30053=CARTESIAN_POINT('Ctrl Pts',(35.9241112984395,-30.0440187000186,-80.4173063663779));
#30054=CARTESIAN_POINT('Ctrl Pts',(35.9184094292111,-30.0433848533287,-80.414328989923));
#30055=CARTESIAN_POINT('Ctrl Pts',(35.9121007299712,-30.0426926542716,-80.4110327898815));
#30056=CARTESIAN_POINT('Ctrl Pts',(35.9054294055848,-30.0419606674906,-80.4075471236796));
#30057=CARTESIAN_POINT('Ctrl Pts',(35.8980797602659,-30.041163498866,-80.4037050603245));
#30058=CARTESIAN_POINT('Ctrl Pts',(35.8900865793965,-30.0403109610116,-80.399523304037));
#30059=CARTESIAN_POINT('Ctrl Pts',(35.8814545114029,-30.0393902806408,-80.3950073040619));
#30060=CARTESIAN_POINT('Ctrl Pts',(35.8720723164423,-30.0384051544974,-80.3900953223086));
#30061=CARTESIAN_POINT('Ctrl Pts',(35.8620410816167,-30.037374348107,-80.384838343375));
#30062=CARTESIAN_POINT('Ctrl Pts',(35.8506994554101,-30.0362088863294,-80.3788946394264));
#30063=CARTESIAN_POINT('Ctrl Pts',(35.8385288432859,-30.0349852883917,-80.3725102391835));
#30064=CARTESIAN_POINT('Ctrl Pts',(35.8257379744632,-30.0337354894307,-80.3657921192093));
#30065=CARTESIAN_POINT('Ctrl Pts',(35.80663504561,-30.0318689375205,-80.3557587297912));
#30066=CARTESIAN_POINT('Ctrl Pts',(35.7861519826339,-30.0299457365785,-80.3449824179376));
#30067=CARTESIAN_POINT('Ctrl Pts',(35.7651021866241,-30.0280668362265,-80.3338856055751));
#30068=CARTESIAN_POINT('Ctrl Pts',(35.7502135775262,-30.0267378821187,-80.3260367835997));
#30069=CARTESIAN_POINT('Ctrl Pts',(35.7350453573012,-30.0254309288662,-80.3180298053536));
#30070=CARTESIAN_POINT('Ctrl Pts',(35.7198657385427,-30.0241719306146,-80.3100055487063));
#30071=CARTESIAN_POINT('Ctrl Pts',(35.7070048572268,-30.0231052485491,-80.303207024051));
#30072=CARTESIAN_POINT('Ctrl Pts',(35.6941363958872,-30.0220728634014,-80.2963964500695));
#30073=CARTESIAN_POINT('Ctrl Pts',(35.6813871324549,-30.0210841167044,-80.2896410310027));
#30074=CARTESIAN_POINT('Ctrl Pts',(35.6696916340288,-30.0201770928986,-80.2834439676601));
#30075=CARTESIAN_POINT('Ctrl Pts',(35.6580968184065,-30.019306721719,-80.277293533371));
#30076=CARTESIAN_POINT('Ctrl Pts',(35.6466609403558,-30.0184755468053,-80.2712210194501));
#30077=CARTESIAN_POINT('Ctrl Pts',(35.6358843219359,-30.0176922877635,-80.2654985760064));
#30078=CARTESIAN_POINT('Ctrl Pts',(35.6252491146204,-30.016943781666,-80.259845481224));
#30079=CARTESIAN_POINT('Ctrl Pts',(35.6147628037156,-30.0162286740995,-80.2542662512699));
#30080=CARTESIAN_POINT('Ctrl Pts',(35.6047424413365,-30.015545341608,-80.2489349287063));
#30081=CARTESIAN_POINT('Ctrl Pts',(35.5948582484425,-30.0148924602529,-80.2436711712074));
#30082=CARTESIAN_POINT('Ctrl Pts',(35.5850744769257,-30.0142662671988,-80.2384565839212));
#30083=CARTESIAN_POINT('Ctrl Pts',(35.5752147659519,-30.0136352137736,-80.2332015221691));
#30084=CARTESIAN_POINT('Ctrl Pts',(35.5654576226954,-30.0130312331291,-80.2279967106397));
#30085=CARTESIAN_POINT('Ctrl Pts',(35.5557161299514,-30.0124483251838,-80.2227966335814));
#30086=CARTESIAN_POINT('Ctrl Pts',(35.5463166337192,-30.011885881503,-80.2177791166565));
#30087=CARTESIAN_POINT('Ctrl Pts',(35.5369237555601,-30.0113425793404,-80.2127617960903));
#30088=CARTESIAN_POINT('Ctrl Pts',(35.527449210758,-30.0108138798861,-80.2076982897044));
#30089=CARTESIAN_POINT('Ctrl Pts',(35.5173854852471,-30.0102523029135,-80.2023199058924));
#30090=CARTESIAN_POINT('Ctrl Pts',(35.5072295820741,-30.0097072585674,-80.1968893857751));
#30091=CARTESIAN_POINT('Ctrl Pts',(35.4969314265015,-30.0091776938893,-80.1913806298767));
#30092=CARTESIAN_POINT('Ctrl Pts',(35.4863013363226,-30.0086310600534,-80.1856943133747));
#30093=CARTESIAN_POINT('Ctrl Pts',(35.4755200531343,-30.0081010145809,-80.179924829647));
#30094=CARTESIAN_POINT('Ctrl Pts',(35.4645869543455,-30.0075897005368,-80.1740723946893));
#30095=CARTESIAN_POINT('Ctrl Pts',(35.4529836026822,-30.0070470404201,-80.1678611766064));
#30096=CARTESIAN_POINT('Ctrl Pts',(35.4412095733346,-30.0065255874064,-80.1615566898743));
#30097=CARTESIAN_POINT('Ctrl Pts',(35.4293193553524,-30.006029968557,-80.155188639105));
#30098=CARTESIAN_POINT('Ctrl Pts',(35.4163900185768,-30.0054910362157,-80.1482640668957));
#30099=CARTESIAN_POINT('Ctrl Pts',(35.4033237830985,-30.0049828032927,-80.1412645884185));
#30100=CARTESIAN_POINT('Ctrl Pts',(35.390248088844,-30.0045114644718,-80.1342590949445));
#30101=CARTESIAN_POINT('Ctrl Pts',(35.3749727023187,-30.0039608334663,-80.1260750843265));
#30102=CARTESIAN_POINT('Ctrl Pts',(35.3596852987564,-30.0034608471724,-80.117883339593));
#30103=CARTESIAN_POINT('Ctrl Pts',(35.3446546541224,-30.0030178726731,-80.1098288811597));
#30104=CARTESIAN_POINT('Ctrl Pts',(35.3255177476667,-30.002453880791,-80.0995740037848));
#30105=CARTESIAN_POINT('Ctrl Pts',(35.3068025013319,-30.0019830567705,-80.0895446150785));
#30106=CARTESIAN_POINT('Ctrl Pts',(35.2891166492053,-30.0016033783673,-80.0800683623363));
#30107=CARTESIAN_POINT('Ctrl Pts',(35.2765328144717,-30.0013332296494,-80.0733258204701));
#30108=CARTESIAN_POINT('Ctrl Pts',(35.2644718949523,-30.001108780868,-80.0668642611809));
#30109=CARTESIAN_POINT('Ctrl Pts',(35.2531305794323,-30.0009240580503,-80.0607896234395));
#30110=CARTESIAN_POINT('Ctrl Pts',(35.2429440867967,-30.0007581445265,-80.055333532168));
#30111=CARTESIAN_POINT('Ctrl Pts',(35.2333387706015,-30.0006241571,-80.0501899303605));
#30112=CARTESIAN_POINT('Ctrl Pts',(35.2244232491389,-30.0005157480259,-80.0454172446047));
#30113=CARTESIAN_POINT('Ctrl Pts',(35.2160963048282,-30.0004144958079,-80.0409596378715));
#30114=CARTESIAN_POINT('Ctrl Pts',(35.2083714999213,-30.0003354840982,-80.0368258108517));
#30115=CARTESIAN_POINT('Ctrl Pts',(35.2012988663028,-30.0002729721797,-80.0330426119596));
#30116=CARTESIAN_POINT('Ctrl Pts',(35.194573831089,-30.0002135325317,-80.0294453457725));
#30117=CARTESIAN_POINT('Ctrl Pts',(35.1884387405858,-30.0001689686332,-80.026165250201));
#30118=CARTESIAN_POINT('Ctrl Pts',(35.1828955521313,-30.0001346028013,-80.0232032990606));
#30119=CARTESIAN_POINT('Ctrl Pts',(35.1772987906466,-30.0000999048353,-80.0202127216702));
#30120=CARTESIAN_POINT('Ctrl Pts',(35.1723061376744,-30.0000755729431,-80.0175468470756));
#30121=CARTESIAN_POINT('Ctrl Pts',(35.1678686123439,-30.0000576033295,-80.0151792621621));
#30122=CARTESIAN_POINT('Ctrl Pts',(35.1638451381212,-30.0000413104023,-80.0130325889241));
#30123=CARTESIAN_POINT('Ctrl Pts',(35.1602777470693,-30.0000302529948,-80.0111309837702));
#30124=CARTESIAN_POINT('Ctrl Pts',(35.1570869279604,-30.0000222392175,-80.0094316687598));
#30125=CARTESIAN_POINT('Ctrl Pts',(35.1539681240623,-30.0000144063073,-80.0077707064497));
#30126=CARTESIAN_POINT('Ctrl Pts',(35.1512092801205,-30.0000094851495,-80.0063031094198));
#30127=CARTESIAN_POINT('Ctrl Pts',(35.1486928450113,-30.0000061645488,-80.0049656980733));
#30128=CARTESIAN_POINT('Ctrl Pts',(35.1462489150872,-30.0000029396235,-80.0036668211031));
#30129=CARTESIAN_POINT('Ctrl Pts',(35.1440337268313,-30.0000012293401,-80.0024907891863));
#30130=CARTESIAN_POINT('Ctrl Pts',(35.1418962367331,-30.0000004600053,-80.0013564737718));
#30131=CARTESIAN_POINT('Ctrl Pts',(35.1410360151499,-30.0000001503906,-80.0008999745336));
#30132=CARTESIAN_POINT('Ctrl Pts',(35.1401878688062,-30.,-80.0004499589203));
#30133=CARTESIAN_POINT('Ctrl Pts',(35.1393398282202,-30.,-80.));
#30134=CARTESIAN_POINT('',(40.3554345327697,-32.0000000029374,-82.));
#30135=CARTESIAN_POINT('Ctrl Pts',(40.3554345313214,-32.0000000046471,-82.));
#30136=CARTESIAN_POINT('Ctrl Pts',(39.8311124520329,-31.5555126118589,-82.0000000010328));
#30137=CARTESIAN_POINT('Ctrl Pts',(38.4326846135015,-30.6269153251775,-81.6648999638687));
#30138=CARTESIAN_POINT('Ctrl Pts',(36.8259962365364,-30.1497856813059,-80.8876206939655));
#30139=CARTESIAN_POINT('Ctrl Pts',(35.9663031078275,-30.0488466897261,-80.4393185174872));
#30140=CARTESIAN_POINT('',(25.7,-32.,-82.));
#30141=CARTESIAN_POINT('Origin',(36.2,-30.,-82.));
#30142=CARTESIAN_POINT('',(-5.8,-30.,-60.5));
#30143=CARTESIAN_POINT('',(-5.8,-30.,-82.));
#30144=CARTESIAN_POINT('',(36.2,-30.,-60.5));
#30145=CARTESIAN_POINT('',(25.7,-30.,-60.5));
#30146=CARTESIAN_POINT('',(36.2,-30.,-79.4330532904862));
#30147=CARTESIAN_POINT('',(36.2,-30.,-82.));
#30148=CARTESIAN_POINT('',(35.6696699141101,-30.,-79.7165266452431));
#30149=CARTESIAN_POINT('Origin',(-5.79999999999999,-37.,-82.));
#30150=CARTESIAN_POINT('',(-12.8,-37.,-60.5));
#30151=CARTESIAN_POINT('',(-12.8,-37.,-82.));
#30152=CARTESIAN_POINT('Origin',(-5.79999999999999,-37.,-60.5));
#30153=CARTESIAN_POINT('Ctrl Pts',(43.1511535430799,-37.2336988749927,-80.4393174835207));
#30154=CARTESIAN_POINT('Ctrl Pts',(43.1518328407262,-37.239484438105,-80.4363004990864));
#30155=CARTESIAN_POINT('Ctrl Pts',(43.1531619914171,-37.251626360285,-80.4299516733943));
#30156=CARTESIAN_POINT('Ctrl Pts',(43.1616022519868,-37.3220234554072,-80.3933108331863));
#30157=CARTESIAN_POINT('Ctrl Pts',(43.1813231191454,-37.5335023841969,-80.2821011062626));
#30158=CARTESIAN_POINT('Ctrl Pts',(43.1946959334339,-37.760715809923,-80.1605544746364));
#30159=CARTESIAN_POINT('Ctrl Pts',(43.2000922890855,-37.9721391005235,-80.0472103209018));
#30160=CARTESIAN_POINT('Ctrl Pts',(43.1998885644922,-38.0426860747344,-80.0095380736286));
#30161=CARTESIAN_POINT('Ctrl Pts',(43.2,-38.0548562141931,-80.0030795017744));
#30162=CARTESIAN_POINT('Ctrl Pts',(43.2,-38.0606601717798,-80.));
#30163=CARTESIAN_POINT('Ctrl Pts',(43.1661027492299,-37.0769409045115,-80.1460536883894));
#30164=CARTESIAN_POINT('Ctrl Pts',(43.1664587837163,-37.0813561272506,-80.1437379532276));
#30165=CARTESIAN_POINT('Ctrl Pts',(43.1670812400941,-37.0893385332148,-80.1395507608468));
#30166=CARTESIAN_POINT('Ctrl Pts',(43.1731116841101,-37.1399593630532,-80.1133008325389));
#30167=CARTESIAN_POINT('Ctrl Pts',(43.1893842943803,-37.3106255658304,-80.0237140789211));
#30168=CARTESIAN_POINT('Ctrl Pts',(43.1981667671395,-37.4734287559457,-79.9363677700901));
#30169=CARTESIAN_POINT('Ctrl Pts',(43.2010845620737,-37.6439974687477,-79.8447395815119));
#30170=CARTESIAN_POINT('Ctrl Pts',(43.1999949346742,-37.6947024038551,-79.8176043851626));
#30171=CARTESIAN_POINT('Ctrl Pts',(43.2,-37.702687116552,-79.8133650160679));
#30172=CARTESIAN_POINT('Ctrl Pts',(43.2,-37.7071067811866,-79.8110177634954));
#30173=CARTESIAN_POINT('Ctrl Pts',(43.1810519553799,-36.9201829340303,-79.852789893258));
#30174=CARTESIAN_POINT('Ctrl Pts',(43.1811995800862,-36.9232120123378,-79.8511897097786));
#30175=CARTESIAN_POINT('Ctrl Pts',(43.1816990397624,-36.9308478545482,-79.8471474812294));
#30176=CARTESIAN_POINT('Ctrl Pts',(43.1844913922431,-36.9707931129032,-79.8259370685621));
#30177=CARTESIAN_POINT('Ctrl Pts',(43.1898784543209,-37.0722287967373,-79.7719437547884));
#30178=CARTESIAN_POINT('Ctrl Pts',(43.1966060738988,-37.2016426465078,-79.7030234840527));
#30179=CARTESIAN_POINT('Ctrl Pts',(43.1989499058728,-37.3029428680724,-79.6490065448319));
#30180=CARTESIAN_POINT('Ctrl Pts',(43.1998185084223,-37.3428746141862,-79.6277190373232));
#30181=CARTESIAN_POINT('Ctrl Pts',(43.2,-37.350518018911,-79.6236505303614));
#30182=CARTESIAN_POINT('Ctrl Pts',(43.2,-37.3535533905933,-79.6220355269908));
#30183=CARTESIAN_POINT('Ctrl Pts',(43.1960011615299,-36.7634249635491,-79.5595260981267));
#30184=CARTESIAN_POINT('Ctrl Pts',(43.196056955755,-36.7650749113605,-79.5586436598417));
#30185=CARTESIAN_POINT('Ctrl Pts',(43.1961660005796,-36.7685385217909,-79.5567913413279));
#30186=CARTESIAN_POINT('Ctrl Pts',(43.1968618855616,-36.7886560431392,-79.5460314243991));
#30187=CARTESIAN_POINT('Ctrl Pts',(43.1984815324142,-36.8491838061983,-79.5136657901732));
#30188=CARTESIAN_POINT('Ctrl Pts',(43.1995668915254,-36.9142231649016,-79.4789020799739));
#30189=CARTESIAN_POINT('Ctrl Pts',(43.2000074643706,-36.974740463544,-79.4465563376873));
#30190=CARTESIAN_POINT('Ctrl Pts',(43.1999908830157,-36.9948855968525,-79.4357877043179));
#30191=CARTESIAN_POINT('Ctrl Pts',(43.2,-36.99834892127,-79.4339360446549));
#30192=CARTESIAN_POINT('Ctrl Pts',(43.2,-37.,-79.4330532904862));
#30193=CARTESIAN_POINT('',(43.2,-38.0606601717798,-80.));
#30194=CARTESIAN_POINT('',(43.1511535430799,-37.2336988749927,-80.4393174835207));
#30195=CARTESIAN_POINT('Ctrl Pts',(43.2,-38.0606601717798,-80.));
#30196=CARTESIAN_POINT('Ctrl Pts',(43.2,-38.0585580345045,-80.0011153657436));
#30197=CARTESIAN_POINT('Ctrl Pts',(43.1999991196284,-38.0564519930821,-80.0022328244847));
#30198=CARTESIAN_POINT('Ctrl Pts',(43.1999970367979,-38.0541736842757,-80.003442789511));
#30199=CARTESIAN_POINT('Ctrl Pts',(43.1999949009836,-38.0518374190072,-80.0046835340753));
#30200=CARTESIAN_POINT('Ctrl Pts',(43.1999915030359,-38.0493201363092,-80.0060214842794));
#30201=CARTESIAN_POINT('Ctrl Pts',(43.1999858311707,-38.0464884913384,-80.0075282877598));
#30202=CARTESIAN_POINT('Ctrl Pts',(43.1999799943212,-38.0435744790187,-80.0090789213846));
#30203=CARTESIAN_POINT('Ctrl Pts',(43.1999717556759,-38.0403276954512,-80.0108082972709));
#30204=CARTESIAN_POINT('Ctrl Pts',(43.1999592405457,-38.0366511722259,-80.0127685612255));
#30205=CARTESIAN_POINT('Ctrl Pts',(43.1999460403082,-38.0327733875892,-80.0148361345771));
#30206=CARTESIAN_POINT('Ctrl Pts',(43.1999280866369,-38.0284175454673,-80.0171605574453));
#30207=CARTESIAN_POINT('Ctrl Pts',(43.1999022340605,-38.0235218920689,-80.0197750903894));
#30208=CARTESIAN_POINT('Ctrl Pts',(43.199875223834,-38.0184070166777,-80.0225066992529));
#30209=CARTESIAN_POINT('Ctrl Pts',(43.1998395772318,-38.0127031149793,-80.0255548701494));
#30210=CARTESIAN_POINT('Ctrl Pts',(43.1997907696175,-38.0063931646268,-80.0289288394644));
#30211=CARTESIAN_POINT('Ctrl Pts',(43.1997391599997,-37.9997209654207,-80.0324965054724));
#30212=CARTESIAN_POINT('Ctrl Pts',(43.1996727937424,-37.9923714094918,-80.0364283067011));
#30213=CARTESIAN_POINT('Ctrl Pts',(43.1995857188577,-37.9843791475729,-80.0407056868288));
#30214=CARTESIAN_POINT('Ctrl Pts',(43.1994916961757,-37.9757491746031,-80.0453243636512));
#30215=CARTESIAN_POINT('Ctrl Pts',(43.1993734426238,-37.966370232625,-80.0503457599974));
#30216=CARTESIAN_POINT('Ctrl Pts',(43.1992237896525,-37.9563431022343,-80.0557156969578));
#30217=CARTESIAN_POINT('Ctrl Pts',(43.1990546438421,-37.9450099019562,-80.0617850875693));
#30218=CARTESIAN_POINT('Ctrl Pts',(43.1988452035161,-37.9328493548553,-80.0682993586189));
#30219=CARTESIAN_POINT('Ctrl Pts',(43.198587751229,-37.9200694326044,-80.0751465277811));
#30220=CARTESIAN_POINT('Ctrl Pts',(43.1982019866816,-37.9009200943861,-80.085406273932));
#30221=CARTESIAN_POINT('Ctrl Pts',(43.1977069524981,-37.8803834507095,-80.0964116738306));
#30222=CARTESIAN_POINT('Ctrl Pts',(43.197096925486,-37.8592784408526,-80.1077212616636));
#30223=CARTESIAN_POINT('Ctrl Pts',(43.1966664800395,-37.8443863865487,-80.1157014994036));
#30224=CARTESIAN_POINT('Ctrl Pts',(43.1961794313092,-37.8292152691087,-80.123831066617));
#30225=CARTESIAN_POINT('Ctrl Pts',(43.1956415410083,-37.8140332294389,-80.1319652977188));
#30226=CARTESIAN_POINT('Ctrl Pts',(43.1951858481994,-37.8011712271138,-80.1388564995349));
#30227=CARTESIAN_POINT('Ctrl Pts',(43.1946938688436,-37.7883019867028,-80.1457507280178));
#30228=CARTESIAN_POINT('Ctrl Pts',(43.1941713808472,-37.7755522397004,-80.1525794999662));
#30229=CARTESIAN_POINT('Ctrl Pts',(43.1936920897984,-37.7638565841932,-80.1588436998935));
#30230=CARTESIAN_POINT('Ctrl Pts',(43.1931872432104,-37.752261854596,-80.1650526234636));
#30231=CARTESIAN_POINT('Ctrl Pts',(43.1926613511862,-37.7408263043073,-80.1711745877421));
#30232=CARTESIAN_POINT('Ctrl Pts',(43.1921657825137,-37.7300501369279,-80.1769435546995));
#30233=CARTESIAN_POINT('Ctrl Pts',(43.1916516129956,-37.7194155911391,-80.1826351629201));
#30234=CARTESIAN_POINT('Ctrl Pts',(43.1911212575987,-37.7089301959593,-80.1882448871515));
#30235=CARTESIAN_POINT('Ctrl Pts',(43.1906144722154,-37.6989107919042,-80.1936053044509));
#30236=CARTESIAN_POINT('Ctrl Pts',(43.1900929784067,-37.689027786831,-80.1988908477045));
#30237=CARTESIAN_POINT('Ctrl Pts',(43.1895564882148,-37.6792455207429,-80.2041200142135));
#30238=CARTESIAN_POINT('Ctrl Pts',(43.1890131220655,-37.6693378796787,-80.209416200636));
#30239=CARTESIAN_POINT('Ctrl Pts',(43.1884544776627,-37.6595342095919,-80.2146542275424));
#30240=CARTESIAN_POINT('Ctrl Pts',(43.1878764060617,-37.649746291343,-80.2198804089122));
#30241=CARTESIAN_POINT('Ctrl Pts',(43.1873214765315,-37.6403502150339,-80.224897369384));
#30242=CARTESIAN_POINT('Ctrl Pts',(43.1867481787444,-37.6309606427782,-80.2299076588121));
#30243=CARTESIAN_POINT('Ctrl Pts',(43.1861507982582,-37.6214895334211,-80.2349574569542));
#30244=CARTESIAN_POINT('Ctrl Pts',(43.1855161554004,-37.6114276515097,-80.2403222427113));
#30245=CARTESIAN_POINT('Ctrl Pts',(43.1848542702677,-37.6012737069304,-80.2457316334819));
#30246=CARTESIAN_POINT('Ctrl Pts',(43.1841604774403,-37.5909778004104,-80.2512114642367));
#30247=CARTESIAN_POINT('Ctrl Pts',(43.1834438932237,-37.5803436689861,-80.2568713097603));
#30248=CARTESIAN_POINT('Ctrl Pts',(43.1826932206741,-37.5695584681891,-80.2626060938773));
#30249=CARTESIAN_POINT('Ctrl Pts',(43.1819064399398,-37.5586217154527,-80.2684154677454));
#30250=CARTESIAN_POINT('Ctrl Pts',(43.181071384863,-37.5470139186443,-80.2745812861624));
#30251=CARTESIAN_POINT('Ctrl Pts',(43.1801955856503,-37.5352357254075,-80.280830944653));
#30252=CARTESIAN_POINT('Ctrl Pts',(43.1792810607772,-37.5233418532755,-80.287134955115));
#30253=CARTESIAN_POINT('Ctrl Pts',(43.1782865132751,-37.5104072451902,-80.2939905782281));
#30254=CARTESIAN_POINT('Ctrl Pts',(43.1772460744086,-37.4973363154097,-80.3009102024579));
#30255=CARTESIAN_POINT('Ctrl Pts',(43.1761688075758,-37.4842568799961,-80.3078259962454));
#30256=CARTESIAN_POINT('Ctrl Pts',(43.1749095786937,-37.4689681861163,-80.3159099425939));
#30257=CARTESIAN_POINT('Ctrl Pts',(43.1735998494352,-37.4536687660359,-80.3239881318433));
#30258=CARTESIAN_POINT('Ctrl Pts',(43.1722651888343,-37.4386284888155,-80.3319187022635));
#30259=CARTESIAN_POINT('Ctrl Pts',(43.1705695650427,-37.419520520939,-80.3419941205958));
#30260=CARTESIAN_POINT('Ctrl Pts',(43.1688336276888,-37.4008362912897,-80.3518282593479));
#30261=CARTESIAN_POINT('Ctrl Pts',(43.1671305083866,-37.3831816360191,-80.3611060273308));
#30262=CARTESIAN_POINT('Ctrl Pts',(43.1659173897706,-37.3706063625547,-80.3677145092148));
#30263=CARTESIAN_POINT('Ctrl Pts',(43.1647215545578,-37.3585552199351,-80.3740398813436));
#30264=CARTESIAN_POINT('Ctrl Pts',(43.1635718404781,-37.3472247949594,-80.3799810880577));
#30265=CARTESIAN_POINT('Ctrl Pts',(43.1625391128302,-37.337047270529,-80.3853177613607));
#30266=CARTESIAN_POINT('Ctrl Pts',(43.161543791978,-37.3274519135831,-80.3903441553375));
#30267=CARTESIAN_POINT('Ctrl Pts',(43.1606047204556,-37.3185472096877,-80.3950052279747));
#30268=CARTESIAN_POINT('Ctrl Pts',(43.1597276141756,-37.3102300884439,-80.3993587367162));
#30269=CARTESIAN_POINT('Ctrl Pts',(43.1588996965264,-37.3025158960185,-80.403393346525));
#30270=CARTESIAN_POINT('Ctrl Pts',(43.1581323377048,-37.2954544790796,-80.4070844482838));
#30271=CARTESIAN_POINT('Ctrl Pts',(43.1574026787078,-37.288739984821,-80.4105942086877));
#30272=CARTESIAN_POINT('Ctrl Pts',(43.1567278498295,-37.2826160035565,-80.4137932380386));
#30273=CARTESIAN_POINT('Ctrl Pts',(43.1561125509306,-37.2770842527928,-80.4166817587702));
#30274=CARTESIAN_POINT('Ctrl Pts',(43.1554921835504,-37.2715069346218,-80.4195940734879));
#30275=CARTESIAN_POINT('Ctrl Pts',(43.1549324406422,-37.2665323396178,-80.422190389511));
#30276=CARTESIAN_POINT('Ctrl Pts',(43.1544314048571,-37.2621113943169,-80.4244972128393));
#30277=CARTESIAN_POINT('Ctrl Pts',(43.153976437465,-37.2580969386355,-80.4265919322684));
#30278=CARTESIAN_POINT('Ctrl Pts',(43.1535698408209,-37.2545387286511,-80.4284480890782));
#30279=CARTESIAN_POINT('Ctrl Pts',(43.1532043757704,-37.2513569700072,-80.4301077382135));
#30280=CARTESIAN_POINT('Ctrl Pts',(43.1528471600527,-37.2482470305038,-80.4317299254958));
#30281=CARTESIAN_POINT('Ctrl Pts',(43.1525292589019,-37.2454969340214,-80.4331642750434));
#30282=CARTESIAN_POINT('Ctrl Pts',(43.1522381265435,-37.2429887872574,-80.4344724355697));
#30283=CARTESIAN_POINT('Ctrl Pts',(43.1519553742399,-37.2405528358604,-80.4357429415494));
#30284=CARTESIAN_POINT('Ctrl Pts',(43.1516978788855,-37.2383452067259,-80.4368943655259));
#30285=CARTESIAN_POINT('Ctrl Pts',(43.1514484584103,-37.2362144518533,-80.4380056097449));
#30286=CARTESIAN_POINT('Ctrl Pts',(43.1513493914683,-37.2353681405421,-80.4384469831588));
#30287=CARTESIAN_POINT('Ctrl Pts',(43.151251533532,-37.2345334575184,-80.4388822756696));
#30288=CARTESIAN_POINT('Ctrl Pts',(43.1511535430799,-37.2336988749927,-80.4393174835207));
#30289=CARTESIAN_POINT('',(43.1960011615299,-36.7634249635491,-79.5595260981267));
#30290=CARTESIAN_POINT('Ctrl Pts',(43.1960011615299,-36.7634249635491,-79.5595260981267));
#30291=CARTESIAN_POINT('Ctrl Pts',(43.1810519553799,-36.9201829340303,-79.852789893258));
#30292=CARTESIAN_POINT('Ctrl Pts',(43.1661027492299,-37.0769409045115,-80.1460536883894));
#30293=CARTESIAN_POINT('Ctrl Pts',(43.1511535430799,-37.2336988749927,-80.4393174835207));
#30294=CARTESIAN_POINT('',(43.2,-37.,-79.4330532904862));
#30295=CARTESIAN_POINT('Ctrl Pts',(43.1960011615299,-36.7634249635491,-79.5595260981267));
#30296=CARTESIAN_POINT('Ctrl Pts',(43.1960292081992,-36.7642543601491,-79.5590825136035));
#30297=CARTESIAN_POINT('Ctrl Pts',(43.1960572612725,-36.7650878480138,-79.5586367430988));
#30298=CARTESIAN_POINT('Ctrl Pts',(43.1960893558137,-36.7660475999897,-79.5581234426306));
#30299=CARTESIAN_POINT('Ctrl Pts',(43.1961226720754,-36.7670438861757,-79.5575906027109));
#30300=CARTESIAN_POINT('Ctrl Pts',(43.1961603389068,-36.7681760453388,-79.5569850937024));
#30301=CARTESIAN_POINT('Ctrl Pts',(43.1962049225249,-36.7695294334656,-79.5562612687486));
#30302=CARTESIAN_POINT('Ctrl Pts',(43.1962515944173,-36.7709462136155,-79.5555035401959));
#30303=CARTESIAN_POINT('Ctrl Pts',(43.1963058394868,-36.772605199104,-79.5546162773086));
#30304=CARTESIAN_POINT('Ctrl Pts',(43.1963685817354,-36.7745522931888,-79.5535749414745));
#30305=CARTESIAN_POINT('Ctrl Pts',(43.1964351400283,-36.7766178114237,-79.5524702705853));
#30306=CARTESIAN_POINT('Ctrl Pts',(43.1965112433384,-36.7790072392282,-79.5511923815391));
#30307=CARTESIAN_POINT('Ctrl Pts',(43.1965959455435,-36.781722253071,-79.5497403980796));
#30308=CARTESIAN_POINT('Ctrl Pts',(43.1966879807209,-36.7846723153569,-79.5481627112273));
#30309=CARTESIAN_POINT('Ctrl Pts',(43.196790129808,-36.7880063129438,-79.5463797305347));
#30310=CARTESIAN_POINT('Ctrl Pts',(43.1968992522861,-36.7916712853237,-79.5444198086112));
#30311=CARTESIAN_POINT('Ctrl Pts',(43.1970274016832,-36.7959752931622,-79.5421181488859));
#30312=CARTESIAN_POINT('Ctrl Pts',(43.1971650771572,-36.8007349526751,-79.5395728962987));
#30313=CARTESIAN_POINT('Ctrl Pts',(43.1973056544371,-36.8058001586425,-79.5368643638209));
#30314=CARTESIAN_POINT('Ctrl Pts',(43.1974945509819,-36.812606378731,-79.5332248537439));
#30315=CARTESIAN_POINT('Ctrl Pts',(43.1976882455755,-36.819958112586,-79.5292938352356));
#30316=CARTESIAN_POINT('Ctrl Pts',(43.1978725056392,-36.827430029207,-79.5252987932737));
#30317=CARTESIAN_POINT('Ctrl Pts',(43.1979954253998,-36.8324145396007,-79.5226337035527));
#30318=CARTESIAN_POINT('Ctrl Pts',(43.198114224774,-36.8374510429814,-79.5199409171317));
#30319=CARTESIAN_POINT('Ctrl Pts',(43.1982264691042,-36.8424364029054,-79.5172755779946));
#30320=CARTESIAN_POINT('Ctrl Pts',(43.1983273034174,-36.8469149840789,-79.5148811796236));
#30321=CARTESIAN_POINT('Ctrl Pts',(43.1984228681419,-36.8513517043665,-79.5125092451843));
#30322=CARTESIAN_POINT('Ctrl Pts',(43.1985126193353,-36.855704757511,-79.5101821187262));
#30323=CARTESIAN_POINT('Ctrl Pts',(43.1985964589664,-36.8597710919664,-79.5080082710417));
#30324=CARTESIAN_POINT('Ctrl Pts',(43.1986752428195,-36.8637640427497,-79.5058737234103));
#30325=CARTESIAN_POINT('Ctrl Pts',(43.1987493965147,-36.8676864149637,-79.5037769662875));
#30326=CARTESIAN_POINT('Ctrl Pts',(43.1988210097374,-36.8714744084558,-79.5017520431281));
#30327=CARTESIAN_POINT('Ctrl Pts',(43.1988883185089,-36.8751961754576,-79.4997625797108));
#30328=CARTESIAN_POINT('Ctrl Pts',(43.1989523298725,-36.8788955650162,-79.4977851230288));
#30329=CARTESIAN_POINT('Ctrl Pts',(43.199018439598,-36.8827162245807,-79.49574284317));
#30330=CARTESIAN_POINT('Ctrl Pts',(43.1990811576252,-36.8865194391444,-79.4937099356785));
#30331=CARTESIAN_POINT('Ctrl Pts',(43.1991415844903,-36.8903775558632,-79.4916477121475));
#30332=CARTESIAN_POINT('Ctrl Pts',(43.1992029440351,-36.8942952220383,-79.4895536585038));
#30333=CARTESIAN_POINT('Ctrl Pts',(43.1992619121571,-36.8982693617107,-79.4874294500976));
#30334=CARTESIAN_POINT('Ctrl Pts',(43.1993184857714,-36.9023233152792,-79.4852625997466));
#30335=CARTESIAN_POINT('Ctrl Pts',(43.1993790270456,-36.9066615835204,-79.4829437823496));
#30336=CARTESIAN_POINT('Ctrl Pts',(43.1994367895758,-36.9110908578823,-79.4805763437083));
#30337=CARTESIAN_POINT('Ctrl Pts',(43.1994909980028,-36.9155857306056,-79.4781738547406));
#30338=CARTESIAN_POINT('Ctrl Pts',(43.1995513398438,-36.9205891758262,-79.475499536093));
#30339=CARTESIAN_POINT('Ctrl Pts',(43.1996072226597,-36.9256732808927,-79.4727821198323));
#30340=CARTESIAN_POINT('Ctrl Pts',(43.1996574096079,-36.9307457718128,-79.4700709151224));
#30341=CARTESIAN_POINT('Ctrl Pts',(43.1997276363855,-36.937843726654,-79.4662771165926));
#30342=CARTESIAN_POINT('Ctrl Pts',(43.1997864800304,-36.9449173141003,-79.4624963497728));
#30343=CARTESIAN_POINT('Ctrl Pts',(43.1998327796822,-36.9516155346497,-79.4589161931795));
#30344=CARTESIAN_POINT('Ctrl Pts',(43.1998710512116,-36.9571523180866,-79.45595681739));
#30345=CARTESIAN_POINT('Ctrl Pts',(43.1999008268764,-36.962427686723,-79.4531371514988));
#30346=CARTESIAN_POINT('Ctrl Pts',(43.1999233926374,-36.9672509968511,-79.4505590813936));
#30347=CARTESIAN_POINT('Ctrl Pts',(43.1999421370943,-36.9712575237635,-79.4484175837531));
#30348=CARTESIAN_POINT('Ctrl Pts',(43.1999559634524,-36.9749512584795,-79.4464432532279));
#30349=CARTESIAN_POINT('Ctrl Pts',(43.1999662322813,-36.9782572558855,-79.4446761449678));
#30350=CARTESIAN_POINT('Ctrl Pts',(43.1999757221302,-36.9813124646361,-79.4430430872376));
#30351=CARTESIAN_POINT('Ctrl Pts',(43.1999821989834,-36.9840359420526,-79.441587320043));
#30352=CARTESIAN_POINT('Ctrl Pts',(43.1999868084131,-36.9864102228559,-79.4403181798015));
#30353=CARTESIAN_POINT('Ctrl Pts',(43.1999909974291,-36.9885679518936,-79.4391647944275));
#30354=CARTESIAN_POINT('Ctrl Pts',(43.1999936526081,-36.99043720414,-79.4381655845785));
#30355=CARTESIAN_POINT('Ctrl Pts',(43.1999954793619,-36.992044567104,-79.4373063422928));
#30356=CARTESIAN_POINT('Ctrl Pts',(43.1999972411365,-36.993594754739,-79.4364776640189));
#30357=CARTESIAN_POINT('Ctrl Pts',(43.1999982338138,-36.9949010490038,-79.4357793353878));
#30358=CARTESIAN_POINT('Ctrl Pts',(43.1999988737606,-36.9960291877518,-79.4351762236091));
#30359=CARTESIAN_POINT('Ctrl Pts',(43.1999994864524,-36.9971092795438,-79.4345987981081));
#30360=CARTESIAN_POINT('Ctrl Pts',(43.1999997736227,-36.9980259236369,-79.4341087287606));
#30361=CARTESIAN_POINT('Ctrl Pts',(43.1999999102358,-36.9988789739787,-79.4336526480419));
#30362=CARTESIAN_POINT('Ctrl Pts',(43.1999999713846,-36.9992608047016,-79.4334485034305));
#30363=CARTESIAN_POINT('Ctrl Pts',(43.2,-36.9996304850866,-79.433250852737));
#30364=CARTESIAN_POINT('Ctrl Pts',(43.2,-37.,-79.4330532904862));
#30365=CARTESIAN_POINT('',(43.2,-37.5303300858899,-79.7165266452431));
#30366=CARTESIAN_POINT('Ctrl Pts',(36.436577026206,-30.0039989057554,-79.5595271622931));
#30367=CARTESIAN_POINT('Ctrl Pts',(36.4332771028451,-30.0038873154276,-79.5577622708323));
#30368=CARTESIAN_POINT('Ctrl Pts',(36.4202666560633,-30.0033694511005,-79.5508025798716));
#30369=CARTESIAN_POINT('Ctrl Pts',(36.3506535373324,-30.0014962059641,-79.5135785874434));
#30370=CARTESIAN_POINT('Ctrl Pts',(36.2859379196174,-30.0004166770606,-79.4789881033753));
#30371=CARTESIAN_POINT('Ctrl Pts',(36.2163534620505,-29.9999221450745,-79.4417960806958));
#30372=CARTESIAN_POINT('Ctrl Pts',(36.2033021852651,-30.,-79.4348188136896));
#30373=CARTESIAN_POINT('Ctrl Pts',(36.2,-30.,-79.4330532904862));
#30374=CARTESIAN_POINT('Ctrl Pts',(36.2798190534131,-30.018948167079,-79.8527909473578));
#30375=CARTESIAN_POINT('Ctrl Pts',(36.2737608688324,-30.0186529125428,-79.8495905657678));
#30376=CARTESIAN_POINT('Ctrl Pts',(36.243977700825,-30.0168261623877,-79.8337978854855));
#30377=CARTESIAN_POINT('Ctrl Pts',(36.1277186009693,-30.0110875261413,-79.7718565459915));
#30378=CARTESIAN_POINT('Ctrl Pts',(35.9986160684372,-30.0048036635674,-79.7031095050481));
#30379=CARTESIAN_POINT('Ctrl Pts',(35.8823679293519,-30.0007586545453,-79.6411504032807));
#30380=CARTESIAN_POINT('Ctrl Pts',(35.8525173806862,-30.,-79.6252655486187));
#30381=CARTESIAN_POINT('Ctrl Pts',(35.8464466094067,-30.,-79.6220355269908));
#30382=CARTESIAN_POINT('Ctrl Pts',(36.1230610806203,-30.0338974284025,-80.1460547324225));
#30383=CARTESIAN_POINT('Ctrl Pts',(36.1142306075048,-30.0331853485277,-80.1414232481978));
#30384=CARTESIAN_POINT('Ctrl Pts',(36.0853799797672,-30.0285249362864,-80.1262758307435));
#30385=CARTESIAN_POINT('Ctrl Pts',(35.8888018779173,-30.0154387041423,-80.0204505126233));
#30386=CARTESIAN_POINT('Ctrl Pts',(35.7271314036452,-30.0041153121472,-79.9346805897903));
#30387=CARTESIAN_POINT('Ctrl Pts',(35.5307249156969,-30.0009916227304,-79.8304584379456));
#30388=CARTESIAN_POINT('Ctrl Pts',(35.5017325761074,-30.,-79.8157122835477));
#30389=CARTESIAN_POINT('Ctrl Pts',(35.4928932188134,-30.,-79.8110177634954));
#30390=CARTESIAN_POINT('Ctrl Pts',(35.9663031078275,-30.0488466897261,-80.4393185174872));
#30391=CARTESIAN_POINT('Ctrl Pts',(35.9547319536141,-30.0474880879196,-80.43328453461));
#30392=CARTESIAN_POINT('Ctrl Pts',(35.9091462718646,-30.0412136289532,-80.4097057710142));
#30393=CARTESIAN_POINT('Ctrl Pts',(35.6659250571246,-30.0184091986823,-80.2818326175006));
#30394=CARTESIAN_POINT('Ctrl Pts',(35.4398443483541,-30.0051041930071,-80.160865945828));
#30395=CARTESIAN_POINT('Ctrl Pts',(35.1967469144272,-29.9990469952302,-80.0305407044586));
#30396=CARTESIAN_POINT('Ctrl Pts',(35.1509477715285,-30.,-80.0061590184768));
#30397=CARTESIAN_POINT('Ctrl Pts',(35.1393398282202,-30.,-80.));
#30398=CARTESIAN_POINT('',(36.436577026206,-30.0039989057554,-79.5595271622931));
#30399=CARTESIAN_POINT('Ctrl Pts',(36.2,-30.,-79.4330532904862));
#30400=CARTESIAN_POINT('Ctrl Pts',(36.2008299527297,-30.,-79.4334970271891));
#30401=CARTESIAN_POINT('Ctrl Pts',(36.2016639947661,-30.0000001318966,-79.4339429495765));
#30402=CARTESIAN_POINT('Ctrl Pts',(36.2026243726041,-30.0000004919523,-79.4344563936253));
#30403=CARTESIAN_POINT('Ctrl Pts',(36.2036213072276,-30.0000008657134,-79.4349893819235));
#30404=CARTESIAN_POINT('Ctrl Pts',(36.2047541916982,-30.0000014834565,-79.4355950301953));
#30405=CARTESIAN_POINT('Ctrl Pts',(36.2061084253782,-30.0000026652048,-79.4363189798766));
#30406=CARTESIAN_POINT('Ctrl Pts',(36.2075260880269,-30.0000039023034,-79.4370768375772));
#30407=CARTESIAN_POINT('Ctrl Pts',(36.2091860867889,-30.0000057563249,-79.4379642132136));
#30408=CARTESIAN_POINT('Ctrl Pts',(36.2111343335543,-30.0000088552473,-79.4390056428516));
#30409=CARTESIAN_POINT('Ctrl Pts',(36.2132010681467,-30.0000121426389,-79.4401104098125));
#30410=CARTESIAN_POINT('Ctrl Pts',(36.2155918667794,-30.0000168376519,-79.4413883725556));
#30411=CARTESIAN_POINT('Ctrl Pts',(36.2183083747451,-30.0000239426542,-79.4428404082484));
#30412=CARTESIAN_POINT('Ctrl Pts',(36.2212600424038,-30.0000316627146,-79.4444181421803));
#30413=CARTESIAN_POINT('Ctrl Pts',(36.2245957852199,-30.0000422506377,-79.4462011421318));
#30414=CARTESIAN_POINT('Ctrl Pts',(36.2282625669554,-30.0000570554247,-79.4481610613737));
#30415=CARTESIAN_POINT('Ctrl Pts',(36.2325685639487,-30.0000744410705,-79.4504626454252));
#30416=CARTESIAN_POINT('Ctrl Pts',(36.2373302697605,-30.0000977058088,-79.4530077767654));
#30417=CARTESIAN_POINT('Ctrl Pts',(36.2423974506242,-30.0001283971647,-79.4557161645737));
#30418=CARTESIAN_POINT('Ctrl Pts',(36.2492077206762,-30.0001696462196,-79.4593562265481));
#30419=CARTESIAN_POINT('Ctrl Pts',(36.2565635895459,-30.0002245428704,-79.4632878753195));
#30420=CARTESIAN_POINT('Ctrl Pts',(36.2640392312156,-30.0002929363533,-79.4672835420005));
#30421=CARTESIAN_POINT('Ctrl Pts',(36.2690254529744,-30.0003385545207,-79.469948634982));
#30422=CARTESIAN_POINT('Ctrl Pts',(36.2740634720143,-30.0003900485922,-79.47264141353));
#30423=CARTESIAN_POINT('Ctrl Pts',(36.2790501104482,-30.0004463656574,-79.4753067399276));
#30424=CARTESIAN_POINT('Ctrl Pts',(36.2835298405669,-30.0004969579065,-79.4777011270678));
#30425=CARTESIAN_POINT('Ctrl Pts',(36.2879675194015,-30.0005514021085,-79.4800730463967));
#30426=CARTESIAN_POINT('Ctrl Pts',(36.2923213334954,-30.0006088285208,-79.4824001569821));
#30427=CARTESIAN_POINT('Ctrl Pts',(36.2963883789083,-30.0006624724802,-79.4845739899082));
#30428=CARTESIAN_POINT('Ctrl Pts',(36.3003818689944,-30.0007186889147,-79.4867085221443));
#30429=CARTESIAN_POINT('Ctrl Pts',(36.3043046120262,-30.0007771468605,-79.488805263923));
#30430=CARTESIAN_POINT('Ctrl Pts',(36.3080929712679,-30.0008336021769,-79.4908301763454));
#30431=CARTESIAN_POINT('Ctrl Pts',(36.31181494728,-30.0008921206218,-79.4928196289511));
#30432=CARTESIAN_POINT('Ctrl Pts',(36.3155143907173,-30.0009531773579,-79.4947970733165));
#30433=CARTESIAN_POINT('Ctrl Pts',(36.3193352828396,-30.0010162385198,-79.4968394350193));
#30434=CARTESIAN_POINT('Ctrl Pts',(36.3231385624469,-30.0010820990913,-79.4988724214067));
#30435=CARTESIAN_POINT('Ctrl Pts',(36.3269965827126,-30.0011521042404,-79.5009347253047));
#30436=CARTESIAN_POINT('Ctrl Pts',(36.3309140786862,-30.0012231885972,-79.5030288219293));
#30437=CARTESIAN_POINT('Ctrl Pts',(36.3348878788047,-30.0012985706632,-79.5051530737463));
#30438=CARTESIAN_POINT('Ctrl Pts',(36.338941318577,-30.001379042269,-79.5073199677846));
#30439=CARTESIAN_POINT('Ctrl Pts',(36.3432790352519,-30.0014651575305,-79.5096388310046));
#30440=CARTESIAN_POINT('Ctrl Pts',(36.3477075574441,-30.0015571244494,-79.5120063157128));
#30441=CARTESIAN_POINT('Ctrl Pts',(36.3522014777422,-30.0016548591704,-79.5144088482003));
#30442=CARTESIAN_POINT('Ctrl Pts',(36.3572038614396,-30.0017636520601,-79.5170832145777));
#30443=CARTESIAN_POINT('Ctrl Pts',(36.3622866553372,-30.0018796258686,-79.5198006753319));
#30444=CARTESIAN_POINT('Ctrl Pts',(36.3673576144516,-30.0020008981935,-79.5225119150777));
#30445=CARTESIAN_POINT('Ctrl Pts',(36.3744533378275,-30.0021705928904,-79.5263057155812));
#30446=CARTESIAN_POINT('Ctrl Pts',(36.3815242557079,-30.002350837276,-79.5300864658661));
#30447=CARTESIAN_POINT('Ctrl Pts',(36.3882195935254,-30.002530930071,-79.5336665752434));
#30448=CARTESIAN_POINT('Ctrl Pts',(36.3937541349189,-30.0026797994866,-79.5366259873123));
#30449=CARTESIAN_POINT('Ctrl Pts',(36.3990271081334,-30.0028283234338,-79.5394456612337));
#30450=CARTESIAN_POINT('Ctrl Pts',(36.403848040124,-30.0029687740773,-79.5420236987559));
#30451=CARTESIAN_POINT('Ctrl Pts',(36.4078525618013,-30.0030854398273,-79.5441651533881));
#30452=CARTESIAN_POINT('Ctrl Pts',(36.4115443102677,-30.003196448923,-79.5461394153452));
#30453=CARTESIAN_POINT('Ctrl Pts',(36.4148484404365,-30.0032979091831,-79.5479064272231));
#30454=CARTESIAN_POINT('Ctrl Pts',(36.4179018188432,-30.0033916695834,-79.5495393398617));
#30455=CARTESIAN_POINT('Ctrl Pts',(36.4206235917814,-30.003477230334,-79.5509949504925));
#30456=CARTESIAN_POINT('Ctrl Pts',(36.4229963509836,-30.0035528568103,-79.5522639251833));
#30457=CARTESIAN_POINT('Ctrl Pts',(36.4251527711832,-30.0036215879571,-79.553417199672));
#30458=CARTESIAN_POINT('Ctrl Pts',(36.4270208459444,-30.0036821028092,-79.5544162805173));
#30459=CARTESIAN_POINT('Ctrl Pts',(36.4286271741609,-30.0037345951404,-79.5552753797164));
#30460=CARTESIAN_POINT('Ctrl Pts',(36.4301763628356,-30.0037852202394,-79.5561039194482));
#30461=CARTESIAN_POINT('Ctrl Pts',(36.4314817914515,-30.0038283717003,-79.5568020965912));
#30462=CARTESIAN_POINT('Ctrl Pts',(36.4326091752435,-30.0038658552317,-79.5574050508185));
#30463=CARTESIAN_POINT('Ctrl Pts',(36.433688544672,-30.0039017423699,-79.5579823257132));
#30464=CARTESIAN_POINT('Ctrl Pts',(36.4346045677364,-30.0039324314054,-79.5584722388144));
#30465=CARTESIAN_POINT('Ctrl Pts',(36.4354570467087,-30.0039611222382,-79.5589281670262));
#30466=CARTESIAN_POINT('Ctrl Pts',(36.4358385180197,-30.0039739609473,-79.5591321879327));
#30467=CARTESIAN_POINT('Ctrl Pts',(36.4362078551915,-30.003986421855,-79.5593297192922));
#30468=CARTESIAN_POINT('Ctrl Pts',(36.4365770262059,-30.0039989057554,-79.5595271622931));
#30469=CARTESIAN_POINT('Ctrl Pts',(35.9663031078275,-30.0488466897261,-80.4393185174872));
#30470=CARTESIAN_POINT('Ctrl Pts',(36.1230610806203,-30.0338974284025,-80.1460547324225));
#30471=CARTESIAN_POINT('Ctrl Pts',(36.2798190534131,-30.018948167079,-79.8527909473578));
#30472=CARTESIAN_POINT('Ctrl Pts',(36.436577026206,-30.0039989057554,-79.5595271622931));
#30473=CARTESIAN_POINT('Ctrl Pts',(35.9663031078275,-30.0488466897261,-80.4393185174872));
#30474=CARTESIAN_POINT('Ctrl Pts',(36.8259962365364,-30.1497856813059,-80.8876206939655));
#30475=CARTESIAN_POINT('Ctrl Pts',(38.4326846135015,-30.6269153251775,-81.6648999638687));
#30476=CARTESIAN_POINT('Ctrl Pts',(39.8311124520329,-31.5555126118589,-82.0000000010328));
#30477=CARTESIAN_POINT('Ctrl Pts',(40.3554345313214,-32.0000000046471,-82.));
#30478=CARTESIAN_POINT('Ctrl Pts',(36.1230610806203,-30.0338974284025,-80.1460547324225));
#30479=CARTESIAN_POINT('Ctrl Pts',(36.9825844189037,-30.1108748191349,-80.598094697917));
#30480=CARTESIAN_POINT('Ctrl Pts',(38.5823256603806,-30.5454841504775,-81.4026214140165));
#30481=CARTESIAN_POINT('Ctrl Pts',(39.962810125821,-31.4492010715984,-81.7954256760992));
#30482=CARTESIAN_POINT('Ctrl Pts',(40.4786184794921,-31.8863889667545,-81.8224303038977));
#30483=CARTESIAN_POINT('Ctrl Pts',(36.2798190534131,-30.018948167079,-79.8527909473578));
#30484=CARTESIAN_POINT('Ctrl Pts',(37.139172601271,-30.0719639569638,-80.3085687018685));
#30485=CARTESIAN_POINT('Ctrl Pts',(38.7319667072597,-30.4640529757775,-81.1403428641643));
#30486=CARTESIAN_POINT('Ctrl Pts',(40.094507799609,-31.3428895313378,-81.5908513511656));
#30487=CARTESIAN_POINT('Ctrl Pts',(40.6018024276628,-31.7727779288618,-81.6448606077953));
#30488=CARTESIAN_POINT('Ctrl Pts',(36.436577026206,-30.0039989057554,-79.5595271622931));
#30489=CARTESIAN_POINT('Ctrl Pts',(37.2957607836383,-30.0330530947928,-80.01904270582));
#30490=CARTESIAN_POINT('Ctrl Pts',(38.8816077541387,-30.3826218010775,-80.8780643143121));
#30491=CARTESIAN_POINT('Ctrl Pts',(40.2262054733971,-31.2365779910773,-81.386277026232));
#30492=CARTESIAN_POINT('Ctrl Pts',(40.7249863758335,-31.6591668909691,-81.467290911693));
#30493=CARTESIAN_POINT('',(40.7249863758329,-31.6591668909686,-81.4672909116929));
#30494=CARTESIAN_POINT('Ctrl Pts',(36.436577026206,-30.0039989057554,-79.5595271622931));
#30495=CARTESIAN_POINT('Ctrl Pts',(37.2957607836383,-30.0330530947928,-80.01904270582));
#30496=CARTESIAN_POINT('Ctrl Pts',(38.8816077541387,-30.3826218010775,-80.8780643143121));
#30497=CARTESIAN_POINT('Ctrl Pts',(40.2262054733971,-31.2365779910773,-81.386277026232));
#30498=CARTESIAN_POINT('Ctrl Pts',(40.7249863758335,-31.6591668909691,-81.467290911693));
#30499=CARTESIAN_POINT('',(40.7249863758329,-31.6591668909686,-81.4672909116929));
#30500=CARTESIAN_POINT('Origin',(36.2,-37.,-81.75));
#30501=CARTESIAN_POINT('',(40.7490523794545,-32.3571428571429,-82.));
#30502=CARTESIAN_POINT('',(41.0989794855664,-32.,-81.5));
#30503=CARTESIAN_POINT('',(40.7490523794545,-32.3571428571429,-82.));
#30504=CARTESIAN_POINT('',(41.2,-32.1010205144336,-81.5));
#30505=CARTESIAN_POINT('Origin',(36.2,-37.,-81.5));
#30506=CARTESIAN_POINT('',(40.8428571428571,-32.4509476205455,-82.));
#30507=CARTESIAN_POINT('',(41.2,-32.1010205144336,-81.5));
#30508=CARTESIAN_POINT('Origin',(36.2,-37.,-82.));
#30509=CARTESIAN_POINT('Ctrl Pts',(40.3554345313208,-32.0000000046466,-82.));
#30510=CARTESIAN_POINT('Ctrl Pts',(40.4919662599274,-32.1157430459277,-82.));
#30511=CARTESIAN_POINT('Ctrl Pts',(40.6227896098978,-32.2334311135731,-82.));
#30512=CARTESIAN_POINT('Ctrl Pts',(40.7490523794545,-32.3571428571429,-82.));
#30513=CARTESIAN_POINT('Ctrl Pts',(40.4786184794915,-31.8863889667539,-81.8224303038976));
#30514=CARTESIAN_POINT('Ctrl Pts',(40.6129332622184,-32.0002312430992,-81.8294622194963));
#30515=CARTESIAN_POINT('Ctrl Pts',(40.7417444835387,-32.1166492773747,-81.8333333333333));
#30516=CARTESIAN_POINT('Ctrl Pts',(40.8656947481584,-32.2380952380952,-81.8333333333333));
#30517=CARTESIAN_POINT('Ctrl Pts',(40.6018024276622,-31.7727779288612,-81.6448606077953));
#30518=CARTESIAN_POINT('Ctrl Pts',(40.7339002645095,-31.8847194402708,-81.6589244389925));
#30519=CARTESIAN_POINT('Ctrl Pts',(40.8606993571796,-31.9998674411764,-81.6666666666667));
#30520=CARTESIAN_POINT('Ctrl Pts',(40.9823371168624,-32.1190476190476,-81.6666666666667));
#30521=CARTESIAN_POINT('Ctrl Pts',(40.7249863758329,-31.6591668909686,-81.4672909116929));
#30522=CARTESIAN_POINT('Ctrl Pts',(40.8548672668006,-31.7692076374424,-81.4883866584888));
#30523=CARTESIAN_POINT('Ctrl Pts',(40.9796542308205,-31.883085604978,-81.5));
#30524=CARTESIAN_POINT('Ctrl Pts',(41.0989794855664,-32.,-81.5));
#30525=CARTESIAN_POINT('Ctrl Pts',(40.7490523794545,-32.3571428571429,-82.));
#30526=CARTESIAN_POINT('Ctrl Pts',(40.6227896098978,-32.2334311135731,-82.));
#30527=CARTESIAN_POINT('Ctrl Pts',(40.4919662599274,-32.1157430459277,-82.));
#30528=CARTESIAN_POINT('Ctrl Pts',(40.3554345313208,-32.0000000046466,-82.));
#30529=CARTESIAN_POINT('Ctrl Pts',(40.7249863758329,-31.6591668909686,-81.4672909116929));
#30530=CARTESIAN_POINT('Ctrl Pts',(40.8548672668006,-31.7692076374424,-81.4883866584888));
#30531=CARTESIAN_POINT('Ctrl Pts',(40.9796542308205,-31.883085604978,-81.5));
#30532=CARTESIAN_POINT('Ctrl Pts',(41.0989794855664,-32.,-81.5));
#30533=CARTESIAN_POINT('Ctrl Pts',(41.1999999953529,-32.8445654686786,-82.));
#30534=CARTESIAN_POINT('Ctrl Pts',(41.6444875838123,-33.3688877787829,-82.0000000010328));
#30535=CARTESIAN_POINT('Ctrl Pts',(42.5730840238607,-34.7673153509566,-81.6649014644068));
#30536=CARTESIAN_POINT('Ctrl Pts',(43.0502156814288,-36.3740133275242,-80.8876157502161));
#30537=CARTESIAN_POINT('Ctrl Pts',(43.1511535430799,-37.2336988749927,-80.4393174835207));
#30538=CARTESIAN_POINT('Ctrl Pts',(41.3136110332456,-32.7213815205079,-81.8224303038976));
#30539=CARTESIAN_POINT('Ctrl Pts',(41.7507991208595,-33.237190101247,-81.7954256642113));
#30540=CARTESIAN_POINT('Ctrl Pts',(42.6545151103675,-34.6176754805104,-81.4026223559956));
#30541=CARTESIAN_POINT('Ctrl Pts',(43.0891261012142,-36.217419896311,-80.5980924994436));
#30542=CARTESIAN_POINT('Ctrl Pts',(43.1661027492299,-37.0769409045115,-80.1460536883894));
#30543=CARTESIAN_POINT('Ctrl Pts',(41.4272220711382,-32.5981975723372,-81.6448606077953));
#30544=CARTESIAN_POINT('Ctrl Pts',(41.8571106579067,-33.1054924237111,-81.5908513273897));
#30545=CARTESIAN_POINT('Ctrl Pts',(42.7359461968743,-34.4680356100643,-81.1403432475844));
#30546=CARTESIAN_POINT('Ctrl Pts',(43.1280365209996,-36.0608264650977,-80.308569248671));
#30547=CARTESIAN_POINT('Ctrl Pts',(43.1810519553799,-36.9201829340303,-79.852789893258));
#30548=CARTESIAN_POINT('Ctrl Pts',(41.5408331090309,-32.4750136241665,-81.467290911693));
#30549=CARTESIAN_POINT('Ctrl Pts',(41.9634221949539,-32.9737947461752,-81.3862769905682));
#30550=CARTESIAN_POINT('Ctrl Pts',(42.8173772833811,-34.3183957396181,-80.8780641391733));
#30551=CARTESIAN_POINT('Ctrl Pts',(43.166946940785,-35.9042330338845,-80.0190459978984));
#30552=CARTESIAN_POINT('Ctrl Pts',(43.1960011615299,-36.7634249635491,-79.5595260981267));
#30553=CARTESIAN_POINT('',(41.1999999970626,-32.8445654672303,-82.));
#30554=CARTESIAN_POINT('Ctrl Pts',(43.1511535430799,-37.2336988749927,-80.4393174835207));
#30555=CARTESIAN_POINT('Ctrl Pts',(43.0502156814288,-36.3740133275242,-80.8876157502161));
#30556=CARTESIAN_POINT('Ctrl Pts',(42.5730840238607,-34.7673153509566,-81.6649014644068));
#30557=CARTESIAN_POINT('Ctrl Pts',(41.6444875838123,-33.3688877787829,-82.0000000010328));
#30558=CARTESIAN_POINT('Ctrl Pts',(41.1999999953529,-32.8445654686786,-82.));
#30559=CARTESIAN_POINT('',(41.5408331090314,-32.4750136241671,-81.4672909116929));
#30560=CARTESIAN_POINT('',(41.1999999970626,-32.8445654672303,-82.));
#30561=CARTESIAN_POINT('Ctrl Pts',(41.5408331090309,-32.4750136241665,-81.467290911693));
#30562=CARTESIAN_POINT('Ctrl Pts',(41.9634221949539,-32.9737947461752,-81.3862769905682));
#30563=CARTESIAN_POINT('Ctrl Pts',(42.8173772833811,-34.3183957396181,-80.8780641391733));
#30564=CARTESIAN_POINT('Ctrl Pts',(43.166946940785,-35.9042330338845,-80.0190459978984));
#30565=CARTESIAN_POINT('Ctrl Pts',(43.1960011615299,-36.7634249635491,-79.5595260981267));
#30566=CARTESIAN_POINT('Ctrl Pts',(40.8428571428571,-32.4509476205455,-82.));
#30567=CARTESIAN_POINT('Ctrl Pts',(40.9665688864269,-32.5772103901022,-82.));
#30568=CARTESIAN_POINT('Ctrl Pts',(41.0842569540723,-32.7080337400726,-82.));
#30569=CARTESIAN_POINT('Ctrl Pts',(41.1999999953534,-32.8445654686792,-82.));
#30570=CARTESIAN_POINT('Ctrl Pts',(40.9619047619048,-32.3343052518416,-81.8333333333333));
#30571=CARTESIAN_POINT('Ctrl Pts',(41.0833507226253,-32.4582555164613,-81.8333333333333));
#30572=CARTESIAN_POINT('Ctrl Pts',(41.1997687569007,-32.5870667377815,-81.8294622194963));
#30573=CARTESIAN_POINT('Ctrl Pts',(41.3136110332461,-32.7213815205085,-81.8224303038976));
#30574=CARTESIAN_POINT('Ctrl Pts',(41.0809523809524,-32.2176628831376,-81.6666666666667));
#30575=CARTESIAN_POINT('Ctrl Pts',(41.2001325588236,-32.3393006428204,-81.6666666666667));
#30576=CARTESIAN_POINT('Ctrl Pts',(41.3152805597292,-32.4660997354905,-81.6589244389925));
#30577=CARTESIAN_POINT('Ctrl Pts',(41.4272220711388,-32.5981975723378,-81.6448606077953));
#30578=CARTESIAN_POINT('Ctrl Pts',(41.2,-32.1010205144336,-81.5));
#30579=CARTESIAN_POINT('Ctrl Pts',(41.316914395022,-32.2203457691795,-81.5));
#30580=CARTESIAN_POINT('Ctrl Pts',(41.4307923625576,-32.3451327331994,-81.4883866584888));
#30581=CARTESIAN_POINT('Ctrl Pts',(41.5408331090314,-32.4750136241671,-81.4672909116929));
#30582=CARTESIAN_POINT('Ctrl Pts',(41.1999999953534,-32.8445654686792,-82.));
#30583=CARTESIAN_POINT('Ctrl Pts',(41.0842569540723,-32.7080337400726,-82.));
#30584=CARTESIAN_POINT('Ctrl Pts',(40.9665688864269,-32.5772103901022,-82.));
#30585=CARTESIAN_POINT('Ctrl Pts',(40.8428571428571,-32.4509476205455,-82.));
#30586=CARTESIAN_POINT('Ctrl Pts',(41.2,-32.1010205144336,-81.5));
#30587=CARTESIAN_POINT('Ctrl Pts',(41.316914395022,-32.2203457691795,-81.5));
#30588=CARTESIAN_POINT('Ctrl Pts',(41.4307923625576,-32.3451327331994,-81.4883866584888));
#30589=CARTESIAN_POINT('Ctrl Pts',(41.5408331090314,-32.4750136241671,-81.4672909116929));
#30590=CARTESIAN_POINT('Origin',(15.2,-53.,-82.));
#30591=CARTESIAN_POINT('',(41.1999999970626,-73.1554345327697,-82.));
#30592=CARTESIAN_POINT('',(41.2,-61.,-82.));
#30593=CARTESIAN_POINT('',(40.8428571428571,-73.5490523794545,-82.));
#30594=CARTESIAN_POINT('Ctrl Pts',(40.8428571428571,-73.5490523794545,-82.));
#30595=CARTESIAN_POINT('Ctrl Pts',(40.9665688864269,-73.4227896098978,-82.));
#30596=CARTESIAN_POINT('Ctrl Pts',(41.0842569540723,-73.2919662599274,-82.));
#30597=CARTESIAN_POINT('Ctrl Pts',(41.1999999953534,-73.1554345313208,-82.));
#30598=CARTESIAN_POINT('',(40.7490523794545,-73.6428571428571,-82.));
#30599=CARTESIAN_POINT('Origin',(36.2,-69.,-82.));
#30600=CARTESIAN_POINT('',(40.3554345327697,-73.9999999970625,-82.));
#30601=CARTESIAN_POINT('Ctrl Pts',(40.3554345313208,-73.9999999953534,-82.));
#30602=CARTESIAN_POINT('Ctrl Pts',(40.4919662599274,-73.8842569540723,-82.));
#30603=CARTESIAN_POINT('Ctrl Pts',(40.6227896098978,-73.7665688864269,-82.));
#30604=CARTESIAN_POINT('Ctrl Pts',(40.7490523794545,-73.6428571428571,-82.));
#30605=CARTESIAN_POINT('',(-9.95543453276968,-73.9999999970625,-82.));
#30606=CARTESIAN_POINT('',(4.7,-74.,-82.));
#30607=CARTESIAN_POINT('',(-10.3490523794545,-73.6428571428571,-82.));
#30608=CARTESIAN_POINT('Ctrl Pts',(-10.3490523794545,-73.6428571428571,
-82.));
#30609=CARTESIAN_POINT('Ctrl Pts',(-10.2227896098978,-73.7665688864269,
-82.));
#30610=CARTESIAN_POINT('Ctrl Pts',(-10.0919662599274,-73.8842569540723,
-82.));
#30611=CARTESIAN_POINT('Ctrl Pts',(-9.95543453132077,-73.9999999953534,
-82.));
#30612=CARTESIAN_POINT('',(-10.4428571428571,-73.5490523794545,-82.));
#30613=CARTESIAN_POINT('Origin',(-5.8,-69.,-82.));
#30614=CARTESIAN_POINT('',(-10.7999999970626,-73.1554345327697,-82.));
#30615=CARTESIAN_POINT('Ctrl Pts',(-10.7999999953534,-73.1554345313208,
-82.));
#30616=CARTESIAN_POINT('Ctrl Pts',(-10.6842569540723,-73.2919662599274,
-82.));
#30617=CARTESIAN_POINT('Ctrl Pts',(-10.5665688864269,-73.4227896098978,
-82.));
#30618=CARTESIAN_POINT('Ctrl Pts',(-10.4428571428571,-73.5490523794545,
-82.));
#30619=CARTESIAN_POINT('',(-10.8,-45.,-82.));
#30620=CARTESIAN_POINT('Origin',(6.2,-75.5,-12.5));
#30621=CARTESIAN_POINT('',(6.7,-76.,-12.5));
#30622=CARTESIAN_POINT('',(6.7,-75.5,-12.));
#30623=CARTESIAN_POINT('',(6.7,-76.,-12.5));
#30624=CARTESIAN_POINT('Origin',(9.2,-75.75,-12.25));
#30625=CARTESIAN_POINT('',(23.7,-76.,-12.5));
#30626=CARTESIAN_POINT('',(9.2,-76.,-12.5));
#30627=CARTESIAN_POINT('',(23.7,-76.,-12.5));
#30628=CARTESIAN_POINT('Origin',(4.7,-75.75,-60.25));
#30629=CARTESIAN_POINT('',(23.7,-76.,-60.5));
#30630=CARTESIAN_POINT('',(36.2,-76.,-60.5));
#30631=CARTESIAN_POINT('',(4.7,-76.,-60.5));
#30632=CARTESIAN_POINT('',(36.2,-76.,-60.5));
#30633=CARTESIAN_POINT('',(24.2,-75.5,-60.));
#30634=CARTESIAN_POINT('Origin',(36.2,-69.,-60.25));
#30635=CARTESIAN_POINT('',(43.2,-69.,-60.5));
#30636=CARTESIAN_POINT('',(43.2,-69.,-60.5));
#30637=CARTESIAN_POINT('Origin',(36.2,-69.,-60.5));
#30638=CARTESIAN_POINT('Origin',(42.95,-61.,-60.25));
#30639=CARTESIAN_POINT('',(43.2,-37.,-60.5));
#30640=CARTESIAN_POINT('',(43.2,-37.,-60.5));
#30641=CARTESIAN_POINT('',(43.2,-61.,-60.5));
#30642=CARTESIAN_POINT('Origin',(36.2,-37.,-60.25));
#30643=CARTESIAN_POINT('',(36.2,-30.,-60.5));
#30644=CARTESIAN_POINT('Origin',(36.2,-37.,-60.5));
#30645=CARTESIAN_POINT('Origin',(25.7,-30.25,-60.25));
#30646=CARTESIAN_POINT('',(-5.8,-30.,-60.5));
#30647=CARTESIAN_POINT('Origin',(-5.79999999999999,-37.,-60.25));
#30648=CARTESIAN_POINT('',(-12.8,-37.,-60.5));
#30649=CARTESIAN_POINT('Origin',(-12.55,-45.,-60.25));
#30650=CARTESIAN_POINT('',(-12.8,-69.,-60.5));
#30651=CARTESIAN_POINT('',(-12.8,-69.,-60.5));
#30652=CARTESIAN_POINT('',(-12.8,-45.,-60.5));
#30653=CARTESIAN_POINT('Origin',(-5.8,-69.,-60.25));
#30654=CARTESIAN_POINT('',(-5.8,-76.,-60.5));
#30655=CARTESIAN_POINT('',(-5.8,-76.,-60.5));
#30656=CARTESIAN_POINT('Origin',(-5.8,-69.,-60.5));
#30657=CARTESIAN_POINT('Origin',(4.7,-75.75,-60.25));
#30658=CARTESIAN_POINT('',(6.7,-76.,-60.5));
#30659=CARTESIAN_POINT('',(4.7,-76.,-60.5));
#30660=CARTESIAN_POINT('',(6.7,-76.,-60.5));
#30661=CARTESIAN_POINT('Origin',(23.95,-75.75,-74.));
#30662=CARTESIAN_POINT('',(23.7,-76.,-74.));
#30663=CARTESIAN_POINT('',(24.2,-75.5,-74.));
#30664=CARTESIAN_POINT('Origin',(6.45,-75.75,-47.));
#30665=CARTESIAN_POINT('',(6.7,-76.,-47.));
#30666=CARTESIAN_POINT('',(6.2,-75.5,-47.));
#30667=CARTESIAN_POINT('Origin',(36.2,-37.,-82.));
#30668=CARTESIAN_POINT('',(43.2,-37.,-82.));
#30669=CARTESIAN_POINT('Origin',(43.2,-69.,-82.));
#30670=CARTESIAN_POINT('',(43.2,-69.,-79.4330532904862));
#30671=CARTESIAN_POINT('',(43.2,-69.,-82.));
#30672=CARTESIAN_POINT('',(43.2,-67.9393398282202,-80.));
#30673=CARTESIAN_POINT('',(43.2,-68.4696699141101,-79.7165266452431));
#30674=CARTESIAN_POINT('',(43.2,-61.,-80.));
#30675=CARTESIAN_POINT('Origin',(36.2,-69.,-82.));
#30676=CARTESIAN_POINT('',(36.2,-76.,-79.4330532904862));
#30677=CARTESIAN_POINT('',(36.2,-76.,-82.));
#30678=CARTESIAN_POINT('',(36.436575036449,-75.99600116153,-79.5595260981257));
#30679=CARTESIAN_POINT('Ctrl Pts',(36.436575036449,-75.99600116153,-79.5595260981258));
#30680=CARTESIAN_POINT('Ctrl Pts',(36.4357456398491,-75.9960292081993,-79.5590825136025));
#30681=CARTESIAN_POINT('Ctrl Pts',(36.4349121519844,-75.9960572612725,-79.5586367430978));
#30682=CARTESIAN_POINT('Ctrl Pts',(36.4339524000084,-75.9960893558137,-79.5581234426296));
#30683=CARTESIAN_POINT('Ctrl Pts',(36.4329561138224,-75.9961226720755,-79.55759060271));
#30684=CARTESIAN_POINT('Ctrl Pts',(36.4318239546593,-75.9961603389068,-79.5569850937014));
#30685=CARTESIAN_POINT('Ctrl Pts',(36.4304705665326,-75.9962049225249,-79.5562612687477));
#30686=CARTESIAN_POINT('Ctrl Pts',(36.4290537863826,-75.9962515944174,-79.555503540195));
#30687=CARTESIAN_POINT('Ctrl Pts',(36.4273948008941,-75.9963058394869,-79.5546162773077));
#30688=CARTESIAN_POINT('Ctrl Pts',(36.4254477068093,-75.9963685817354,-79.5535749414736));
#30689=CARTESIAN_POINT('Ctrl Pts',(36.4233821885744,-75.9964351400283,-79.5524702705845));
#30690=CARTESIAN_POINT('Ctrl Pts',(36.4209927607699,-75.9965112433385,-79.5511923815383));
#30691=CARTESIAN_POINT('Ctrl Pts',(36.4182777469271,-75.9965959455435,-79.5497403980789));
#30692=CARTESIAN_POINT('Ctrl Pts',(36.4153276846412,-75.9966879807209,-79.5481627112266));
#30693=CARTESIAN_POINT('Ctrl Pts',(36.4119936870543,-75.996790129808,-79.5463797305341));
#30694=CARTESIAN_POINT('Ctrl Pts',(36.4083287146744,-75.9968992522861,-79.5444198086106));
#30695=CARTESIAN_POINT('Ctrl Pts',(36.4040247068359,-75.9970274016833,-79.5421181488853));
#30696=CARTESIAN_POINT('Ctrl Pts',(36.3992650473229,-75.9971650771572,-79.5395728962982));
#30697=CARTESIAN_POINT('Ctrl Pts',(36.3941998413555,-75.9973056544371,-79.5368643638204));
#30698=CARTESIAN_POINT('Ctrl Pts',(36.3873936212671,-75.997494550982,-79.5332248537436));
#30699=CARTESIAN_POINT('Ctrl Pts',(36.3800418874122,-75.9976882455756,-79.5292938352354));
#30700=CARTESIAN_POINT('Ctrl Pts',(36.3725699707913,-75.9978725056392,-79.5252987932736));
#30701=CARTESIAN_POINT('Ctrl Pts',(36.3675854603976,-75.9979954253998,-79.5226337035528));
#30702=CARTESIAN_POINT('Ctrl Pts',(36.3625489570169,-75.9981142247741,-79.5199409171318));
#30703=CARTESIAN_POINT('Ctrl Pts',(36.3575635970929,-75.9982264691042,-79.5172755779947));
#30704=CARTESIAN_POINT('Ctrl Pts',(36.3530850159194,-75.9983273034174,-79.5148811796238));
#30705=CARTESIAN_POINT('Ctrl Pts',(36.3486482956318,-75.998422868142,-79.5125092451845));
#30706=CARTESIAN_POINT('Ctrl Pts',(36.3442952424874,-75.9985126193353,-79.5101821187264));
#30707=CARTESIAN_POINT('Ctrl Pts',(36.340228908032,-75.9985964589664,-79.508008271042));
#30708=CARTESIAN_POINT('Ctrl Pts',(36.3362359572487,-75.9986752428195,-79.5058737234106));
#30709=CARTESIAN_POINT('Ctrl Pts',(36.3323135850348,-75.9987493965147,-79.5037769662878));
#30710=CARTESIAN_POINT('Ctrl Pts',(36.3285255915427,-75.9988210097374,-79.5017520431284));
#30711=CARTESIAN_POINT('Ctrl Pts',(36.324803824541,-75.9988883185089,-79.4997625797111));
#30712=CARTESIAN_POINT('Ctrl Pts',(36.3211044349824,-75.9989523298725,-79.4977851230291));
#30713=CARTESIAN_POINT('Ctrl Pts',(36.3172837754179,-75.9990184395981,-79.4957428431703));
#30714=CARTESIAN_POINT('Ctrl Pts',(36.3134805608543,-75.9990811576252,-79.4937099356788));
#30715=CARTESIAN_POINT('Ctrl Pts',(36.3096224441355,-75.9991415844903,-79.4916477121478));
#30716=CARTESIAN_POINT('Ctrl Pts',(36.3057047779605,-75.9992029440351,-79.4895536585041));
#30717=CARTESIAN_POINT('Ctrl Pts',(36.301730638288,-75.9992619121571,-79.4874294500978));
#30718=CARTESIAN_POINT('Ctrl Pts',(36.2976766847196,-75.9993184857715,-79.4852625997468));
#30719=CARTESIAN_POINT('Ctrl Pts',(36.2933384164784,-75.9993790270456,-79.4829437823498));
#30720=CARTESIAN_POINT('Ctrl Pts',(36.2889091421166,-75.9994367895758,-79.4805763437085));
#30721=CARTESIAN_POINT('Ctrl Pts',(36.2844142693933,-75.9994909980028,-79.4781738547408));
#30722=CARTESIAN_POINT('Ctrl Pts',(36.2794108241728,-75.9995513398438,-79.4754995360931));
#30723=CARTESIAN_POINT('Ctrl Pts',(36.2743267191064,-75.9996072226597,-79.4727821198323));
#30724=CARTESIAN_POINT('Ctrl Pts',(36.2692542281862,-75.9996574096079,-79.4700709151225));
#30725=CARTESIAN_POINT('Ctrl Pts',(36.262156273345,-75.9997276363855,-79.4662771165925));
#30726=CARTESIAN_POINT('Ctrl Pts',(36.2550826858987,-75.9997864800304,-79.4624963497726));
#30727=CARTESIAN_POINT('Ctrl Pts',(36.2483844653493,-75.9998327796822,-79.4589161931793));
#30728=CARTESIAN_POINT('Ctrl Pts',(36.2428476819125,-75.9998710512116,-79.4559568173898));
#30729=CARTESIAN_POINT('Ctrl Pts',(36.2375723132762,-75.9999008268764,-79.4531371514986));
#30730=CARTESIAN_POINT('Ctrl Pts',(36.2327490031482,-75.9999233926374,-79.4505590813934));
#30731=CARTESIAN_POINT('Ctrl Pts',(36.2287424762358,-75.9999421370944,-79.4484175837529));
#30732=CARTESIAN_POINT('Ctrl Pts',(36.2250487415199,-75.9999559634524,-79.4464432532277));
#30733=CARTESIAN_POINT('Ctrl Pts',(36.221742744114,-75.9999662322813,-79.4446761449676));
#30734=CARTESIAN_POINT('Ctrl Pts',(36.2186875353634,-75.9999757221302,-79.4430430872375));
#30735=CARTESIAN_POINT('Ctrl Pts',(36.2159640579471,-75.9999821989834,-79.4415873200428));
#30736=CARTESIAN_POINT('Ctrl Pts',(36.2135897771439,-75.9999868084131,-79.4403181798014));
#30737=CARTESIAN_POINT('Ctrl Pts',(36.2114320481061,-75.9999909974291,-79.4391647944274));
#30738=CARTESIAN_POINT('Ctrl Pts',(36.2095627958598,-75.9999936526082,-79.4381655845784));
#30739=CARTESIAN_POINT('Ctrl Pts',(36.2079554328958,-75.9999954793619,-79.4373063422927));
#30740=CARTESIAN_POINT('Ctrl Pts',(36.2064052452609,-75.9999972411365,-79.4364776640188));
#30741=CARTESIAN_POINT('Ctrl Pts',(36.2050989509961,-75.9999982338138,-79.4357793353877));
#30742=CARTESIAN_POINT('Ctrl Pts',(36.2039708122481,-75.9999988737606,-79.4351762236091));
#30743=CARTESIAN_POINT('Ctrl Pts',(36.2028907204561,-75.9999994864524,-79.434598798108));
#30744=CARTESIAN_POINT('Ctrl Pts',(36.2019740763631,-75.9999997736227,-79.4341087287605));
#30745=CARTESIAN_POINT('Ctrl Pts',(36.2011210260212,-75.9999999102358,-79.4336526480419));
#30746=CARTESIAN_POINT('Ctrl Pts',(36.2007391952983,-75.9999999713846,-79.4334485034305));
#30747=CARTESIAN_POINT('Ctrl Pts',(36.2003695149134,-76.,-79.433250852737));
#30748=CARTESIAN_POINT('Ctrl Pts',(36.2,-76.,-79.4330532904862));
#30749=CARTESIAN_POINT('',(40.7249863758329,-74.3408331090314,-81.4672909116929));
#30750=CARTESIAN_POINT('Ctrl Pts',(40.7249863758336,-74.3408331090309,-81.467290911693));
#30751=CARTESIAN_POINT('Ctrl Pts',(40.2262052538249,-74.7634221949538,-81.3862769905682));
#30752=CARTESIAN_POINT('Ctrl Pts',(38.8816003633081,-75.6173708426798,-80.8780690735046));
#30753=CARTESIAN_POINT('Ctrl Pts',(37.2957669697243,-75.9669469406632,-80.0190459998239));
#30754=CARTESIAN_POINT('Ctrl Pts',(36.436575036449,-75.99600116153,-79.5595260981257));
#30755=CARTESIAN_POINT('',(41.0989794855664,-74.,-81.5));
#30756=CARTESIAN_POINT('Ctrl Pts',(41.0989794855664,-74.,-81.5));
#30757=CARTESIAN_POINT('Ctrl Pts',(40.9796542308205,-74.116914395022,-81.5));
#30758=CARTESIAN_POINT('Ctrl Pts',(40.8548672668006,-74.2307923625576,-81.4883866584888));
#30759=CARTESIAN_POINT('Ctrl Pts',(40.7249863758329,-74.3408331090314,-81.4672909116929));
#30760=CARTESIAN_POINT('',(41.2,-73.8989794855663,-81.5));
#30761=CARTESIAN_POINT('Origin',(36.2,-69.,-81.5));
#30762=CARTESIAN_POINT('',(41.5408331090314,-73.5249863758329,-81.4672909116929));
#30763=CARTESIAN_POINT('Ctrl Pts',(41.5408331090314,-73.5249863758329,-81.4672909116929));
#30764=CARTESIAN_POINT('Ctrl Pts',(41.4307923625576,-73.6548672668006,-81.4883866584888));
#30765=CARTESIAN_POINT('Ctrl Pts',(41.316914395022,-73.7796542308205,-81.5));
#30766=CARTESIAN_POINT('Ctrl Pts',(41.2,-73.8989794855663,-81.5));
#30767=CARTESIAN_POINT('',(43.196001093997,-69.2365770335277,-79.5595271661901));
#30768=CARTESIAN_POINT('Ctrl Pts',(43.196001093997,-69.2365770335277,-79.5595271661901));
#30769=CARTESIAN_POINT('Ctrl Pts',(43.1842694008473,-69.583503938841,-79.745073401727));
#30770=CARTESIAN_POINT('Ctrl Pts',(43.1462431487229,-69.9376909822518,-79.9350664222934));
#30771=CARTESIAN_POINT('Ctrl Pts',(43.0133707147083,-70.6455291845094,-80.3070714285095));
#30772=CARTESIAN_POINT('Ctrl Pts',(42.9185207631589,-70.9987198029951,-80.4888139716367));
#30773=CARTESIAN_POINT('Ctrl Pts',(42.6430856463133,-71.774189502708,-80.8664236862814));
#30774=CARTESIAN_POINT('Ctrl Pts',(42.4467748697811,-72.1911770437546,-81.0543062210682));
#30775=CARTESIAN_POINT('Ctrl Pts',(42.0361750904884,-72.8808297721556,-81.3118311224916));
#30776=CARTESIAN_POINT('Ctrl Pts',(41.8365825645193,-73.1647230633842,-81.398907956803));
#30777=CARTESIAN_POINT('Ctrl Pts',(41.5946015244113,-73.4609452952567,-81.4563646461124));
#30778=CARTESIAN_POINT('Ctrl Pts',(41.5678336290056,-73.4931177116952,-81.4621146824234));
#30779=CARTESIAN_POINT('Ctrl Pts',(41.5408331090314,-73.524986375833,-81.4672909116929));
#30780=CARTESIAN_POINT('Ctrl Pts',(43.2,-69.,-79.4330532904862));
#30781=CARTESIAN_POINT('Ctrl Pts',(43.2,-69.000829952749,-79.4334970271994));
#30782=CARTESIAN_POINT('Ctrl Pts',(43.1999998681034,-69.0016639948047,-79.4339429495971));
#30783=CARTESIAN_POINT('Ctrl Pts',(43.1999995080477,-69.002624372665,-79.4344563936532));
#30784=CARTESIAN_POINT('Ctrl Pts',(43.1999991342865,-69.0036213073114,-79.4349893819589));
#30785=CARTESIAN_POINT('Ctrl Pts',(43.1999985165435,-69.004754191808,-79.4355950302349));
#30786=CARTESIAN_POINT('Ctrl Pts',(43.199997334795,-69.0061084255198,-79.4363189799149));
#30787=CARTESIAN_POINT('Ctrl Pts',(43.1999960976964,-69.0075260882013,-79.4370768376138));
#30788=CARTESIAN_POINT('Ctrl Pts',(43.1999942436748,-69.0091860870021,-79.4379642132424));
#30789=CARTESIAN_POINT('Ctrl Pts',(43.1999911447523,-69.0111343338152,-79.4390056428645));
#30790=CARTESIAN_POINT('Ctrl Pts',(43.1999878573605,-69.0132010684564,-79.4401104098078));
#30791=CARTESIAN_POINT('Ctrl Pts',(43.1999831623473,-69.0155918671473,-79.4413883725242));
#30792=CARTESIAN_POINT('Ctrl Pts',(43.1999760573446,-69.0183083751824,-79.4428404081803));
#30793=CARTESIAN_POINT('Ctrl Pts',(43.1999683372839,-69.021260042912,-79.4444181420698));
#30794=CARTESIAN_POINT('Ctrl Pts',(43.1999577493602,-69.0245957858112,-79.4462011419664));
#30795=CARTESIAN_POINT('Ctrl Pts',(43.1999429445725,-69.0282625676438,-79.4481610611418));
#30796=CARTESIAN_POINT('Ctrl Pts',(43.199925558926,-69.0325685647166,-79.4504626450966));
#30797=CARTESIAN_POINT('Ctrl Pts',(43.1999022941867,-69.0373302706198,-79.45300777632));
#30798=CARTESIAN_POINT('Ctrl Pts',(43.1998716028295,-69.0423974515914,-79.4557161639972));
#30799=CARTESIAN_POINT('Ctrl Pts',(43.1998303537707,-69.0492077221319,-79.4593562259793));
#30800=CARTESIAN_POINT('Ctrl Pts',(43.1997754571138,-69.0565635915756,-79.463287874762));
#30801=CARTESIAN_POINT('Ctrl Pts',(43.1997070636227,-69.0640392338423,-79.4672835414457));
#30802=CARTESIAN_POINT('Ctrl Pts',(43.1996614454515,-69.0690254558109,-79.4699486343282));
#30803=CARTESIAN_POINT('Ctrl Pts',(43.1996099513757,-69.0740634750665,-79.4726414127713));
#30804=CARTESIAN_POINT('Ctrl Pts',(43.1995536343056,-69.0790501137166,-79.4753067390646));
#30805=CARTESIAN_POINT('Ctrl Pts',(43.1995030420523,-69.0835298440296,-79.4777011261113));
#30806=CARTESIAN_POINT('Ctrl Pts',(43.1994485978457,-69.0879675230588,-79.4800730453471));
#30807=CARTESIAN_POINT('Ctrl Pts',(43.1993911714285,-69.0923213373425,-79.4824001558459));
#30808=CARTESIAN_POINT('Ctrl Pts',(43.1993375274645,-69.0963883829329,-79.4845739886913));
#30809=CARTESIAN_POINT('Ctrl Pts',(43.1992813110251,-69.1003818731923,-79.4867085208521));
#30810=CARTESIAN_POINT('Ctrl Pts',(43.1992228530745,-69.1043046163885,-79.4888052625672));
#30811=CARTESIAN_POINT('Ctrl Pts',(43.1991663977533,-69.1080929757928,-79.4908301749301));
#30812=CARTESIAN_POINT('Ctrl Pts',(43.1991078793036,-69.1118149519592,-79.492819627487));
#30813=CARTESIAN_POINT('Ctrl Pts',(43.1990468225626,-69.1155143955378,-79.4947970718204));
#30814=CARTESIAN_POINT('Ctrl Pts',(43.1989837613951,-69.1193352878333,-79.4968394335048));
#30815=CARTESIAN_POINT('Ctrl Pts',(43.1989179008181,-69.1231385675992,-79.4988724198917));
#30816=CARTESIAN_POINT('Ctrl Pts',(43.1988478956635,-69.1269965880092,-79.5009347238157));
#30817=CARTESIAN_POINT('Ctrl Pts',(43.1987768113019,-69.1309140840829,-79.503028820442));
#30818=CARTESIAN_POINT('Ctrl Pts',(43.1987014292312,-69.1348878842858,-79.5051530722874));
#30819=CARTESIAN_POINT('Ctrl Pts',(43.1986209576208,-69.1389413241276,-79.5073199663836));
#30820=CARTESIAN_POINT('Ctrl Pts',(43.1985348423545,-69.1432790408708,-79.5096388296623));
#30821=CARTESIAN_POINT('Ctrl Pts',(43.198442875431,-69.1477075631141,-79.5120063144628));
#30822=CARTESIAN_POINT('Ctrl Pts',(43.1983451407054,-69.1522014834505,-79.5144088470743));
#30823=CARTESIAN_POINT('Ctrl Pts',(43.1982363478113,-69.1572038671642,-79.5170832135758));
#30824=CARTESIAN_POINT('Ctrl Pts',(43.1981203739986,-69.1622866610613,-79.5198006744928));
#30825=CARTESIAN_POINT('Ctrl Pts',(43.1979991016698,-69.1673576201683,-79.5225119144323));
#30826=CARTESIAN_POINT('Ctrl Pts',(43.1978294069763,-69.1744533431577,-79.5263057150058));
#30827=CARTESIAN_POINT('Ctrl Pts',(43.1976491625957,-69.1815242606409,-79.5300864654225));
#30828=CARTESIAN_POINT('Ctrl Pts',(43.197469069805,-69.1882195981374,-79.53366657499));
#30829=CARTESIAN_POINT('Ctrl Pts',(43.1973202003778,-69.193754139822,-79.5366259875136));
#30830=CARTESIAN_POINT('Ctrl Pts',(43.1971716764186,-69.1990271133279,-79.5394456619014));
#30831=CARTESIAN_POINT('Ctrl Pts',(43.1970312257634,-69.2038480455935,-79.5420236998639));
#30832=CARTESIAN_POINT('Ctrl Pts',(43.1969145600064,-69.2078525674018,-79.5441651548097));
#30833=CARTESIAN_POINT('Ctrl Pts',(43.1968035509037,-69.211544316003,-79.5461394170704));
#30834=CARTESIAN_POINT('Ctrl Pts',(43.1967020906367,-69.2148484463065,-79.5479064292267));
#30835=CARTESIAN_POINT('Ctrl Pts',(43.1966083302274,-69.217901824921,-79.5495393421672));
#30836=CARTESIAN_POINT('Ctrl Pts',(43.1965227694685,-69.2206235980485,-79.5509949530684));
#30837=CARTESIAN_POINT('Ctrl Pts',(43.1964471429847,-69.222996357416,-79.5522639279894));
#30838=CARTESIAN_POINT('Ctrl Pts',(43.1963784118337,-69.2251527776853,-79.5534172026444));
#30839=CARTESIAN_POINT('Ctrl Pts',(43.1963178969775,-69.227020852518,-79.5544162836341));
#30840=CARTESIAN_POINT('Ctrl Pts',(43.1962654046425,-69.2286271808036,-79.5552753829538));
#30841=CARTESIAN_POINT('Ctrl Pts',(43.1962147795399,-69.2301763695442,-79.5561039228016));
#30842=CARTESIAN_POINT('Ctrl Pts',(43.1961716280756,-69.2314817982239,-79.5568021000383));
#30843=CARTESIAN_POINT('Ctrl Pts',(43.1961341445413,-69.2326091820715,-79.5574050543386));
#30844=CARTESIAN_POINT('Ctrl Pts',(43.1960982574003,-69.2336885515516,-79.5579823293022));
#30845=CARTESIAN_POINT('Ctrl Pts',(43.1960675683624,-69.2346045746604,-79.5584722424537));
#30846=CARTESIAN_POINT('Ctrl Pts',(43.1960388775278,-69.235457053662,-79.5589281707014));
#30847=CARTESIAN_POINT('Ctrl Pts',(43.1960260388139,-69.235838525103,-79.5591321916864));
#30848=CARTESIAN_POINT('Ctrl Pts',(43.1960135779018,-69.2362078623941,-79.5593297231176));
#30849=CARTESIAN_POINT('Ctrl Pts',(43.196001093997,-69.2365770335277,-79.5595271661901));
#30850=CARTESIAN_POINT('Origin',(6.2,-74.,-12.));
#30851=CARTESIAN_POINT('Origin',(24.2,-74.,-66.));
#30852=CARTESIAN_POINT('Ctrl Pts',(-12.7511535426466,-68.7663011286799,
-80.439317485445));
#30853=CARTESIAN_POINT('Ctrl Pts',(-12.7518328402883,-68.7605155655161,
-80.436300501045));
#30854=CARTESIAN_POINT('Ctrl Pts',(-12.7531619882646,-68.7483736401701,
-80.429951673639));
#30855=CARTESIAN_POINT('Ctrl Pts',(-12.7616022324007,-68.6779765362022,
-80.3933108325196));
#30856=CARTESIAN_POINT('Ctrl Pts',(-12.7813230871559,-68.4664975829723,
-80.2821011164068));
#30857=CARTESIAN_POINT('Ctrl Pts',(-12.7946958959366,-68.2392841615299,
-80.1605544743685));
#30858=CARTESIAN_POINT('Ctrl Pts',(-12.8000922661796,-68.027860897069,-80.0472103201213));
#30859=CARTESIAN_POINT('Ctrl Pts',(-12.7998885602897,-67.9573139240965,
-80.009538072929));
#30860=CARTESIAN_POINT('Ctrl Pts',(-12.8,-67.9451437858327,-80.0030795017881));
#30861=CARTESIAN_POINT('Ctrl Pts',(-12.8,-67.9393398282202,-80.));
#30862=CARTESIAN_POINT('Ctrl Pts',(-12.7661027489825,-68.9230590967111,
-80.1460536890198));
#30863=CARTESIAN_POINT('Ctrl Pts',(-12.7664587807622,-68.9186438738067,
-80.1437379536791));
#30864=CARTESIAN_POINT('Ctrl Pts',(-12.7670812297361,-68.9106614644948,
-80.1395507592229));
#30865=CARTESIAN_POINT('Ctrl Pts',(-12.7731116474475,-68.8600406255686,
-80.1133008293174));
#30866=CARTESIAN_POINT('Ctrl Pts',(-12.7893842443182,-68.6893743987912,
-80.0237140866894));
#30867=CARTESIAN_POINT('Ctrl Pts',(-12.7981667187387,-68.5265712141199,
-79.9363677684688));
#30868=CARTESIAN_POINT('Ctrl Pts',(-12.8010845357288,-68.3560025283503,
-79.8447395802743));
#30869=CARTESIAN_POINT('Ctrl Pts',(-12.7999949300586,-68.3052975948829,
-79.8176043843904));
#30870=CARTESIAN_POINT('Ctrl Pts',(-12.8,-68.2973128834566,-79.8133650160724));
#30871=CARTESIAN_POINT('Ctrl Pts',(-12.8,-68.2928932188135,-79.8110177634954));
#30872=CARTESIAN_POINT('Ctrl Pts',(-12.7810519553184,-69.0798170647423,
-79.8527898925946));
#30873=CARTESIAN_POINT('Ctrl Pts',(-12.7811995792466,-69.0767879864804,
-79.8511897091324));
#30874=CARTESIAN_POINT('Ctrl Pts',(-12.7816990370264,-69.0691521434825,
-79.8471474801494));
#30875=CARTESIAN_POINT('Ctrl Pts',(-12.7844913839459,-69.0292068834798,
-79.8259370670281));
#30876=CARTESIAN_POINT('Ctrl Pts',(-12.7898784436764,-68.927771195494,-79.7719437530437));
#30877=CARTESIAN_POINT('Ctrl Pts',(-12.79660606409,-68.7983573463475,-79.7030234814484));
#30878=CARTESIAN_POINT('Ctrl Pts',(-12.7989499010098,-68.6970571314706,
-79.649006544579));
#30879=CARTESIAN_POINT('Ctrl Pts',(-12.7998185075757,-68.6571253855047,
-79.6277190371445));
#30880=CARTESIAN_POINT('Ctrl Pts',(-12.8,-68.6494819810805,-79.6236505303568));
#30881=CARTESIAN_POINT('Ctrl Pts',(-12.8,-68.6464466094067,-79.6220355269908));
#30882=CARTESIAN_POINT('Ctrl Pts',(-12.7960011616543,-69.2365750327735,
-79.5595260961694));
#30883=CARTESIAN_POINT('Ctrl Pts',(-12.7960569558779,-69.2349250849804,
-79.5586436579119));
#30884=CARTESIAN_POINT('Ctrl Pts',(-12.7961660004731,-69.2314614737188,
-79.5567913389998));
#30885=CARTESIAN_POINT('Ctrl Pts',(-12.796861884166,-69.2113439506909,-79.5460314217622));
#30886=CARTESIAN_POINT('Ctrl Pts',(-12.7984815301387,-69.1508161838819,
-79.513665787615));
#30887=CARTESIAN_POINT('Ctrl Pts',(-12.7995668885118,-69.0857768265977,
-79.4789020769686));
#30888=CARTESIAN_POINT('Ctrl Pts',(-12.8000074624845,-69.0252595353931,
-79.4465563372793));
#30889=CARTESIAN_POINT('Ctrl Pts',(-12.799990882671,-69.0051144027225,-79.4357877041059));
#30890=CARTESIAN_POINT('Ctrl Pts',(-12.8,-69.0016510787044,-79.4339360446411));
#30891=CARTESIAN_POINT('Ctrl Pts',(-12.8,-69.,-79.4330532904862));
#30892=CARTESIAN_POINT('',(-12.8,-67.9393398282202,-80.));
#30893=CARTESIAN_POINT('',(-12.7511535426466,-68.7663011286799,-80.439317485445));
#30894=CARTESIAN_POINT('Ctrl Pts',(-12.8,-67.9393398282202,-80.));
#30895=CARTESIAN_POINT('Ctrl Pts',(-12.8,-67.9414419655024,-80.0011153657472));
#30896=CARTESIAN_POINT('Ctrl Pts',(-12.7999991196284,-67.9435480069317,
-80.0022328244921));
#30897=CARTESIAN_POINT('Ctrl Pts',(-12.7999970367979,-67.9458263157412,
-80.0034427895298));
#30898=CARTESIAN_POINT('Ctrl Pts',(-12.7999949009835,-67.9481625810128,
-80.0046835341056));
#30899=CARTESIAN_POINT('Ctrl Pts',(-12.7999915030358,-67.95067986371,-80.0060214843292));
#30900=CARTESIAN_POINT('Ctrl Pts',(-12.7999858311703,-67.9535115086725,
-80.0075282878437));
#30901=CARTESIAN_POINT('Ctrl Pts',(-12.7999799943207,-67.9564255209836,
-80.0090789215036));
#30902=CARTESIAN_POINT('Ctrl Pts',(-12.7999717556751,-67.9596723045347,
-80.0108082974406));
#30903=CARTESIAN_POINT('Ctrl Pts',(-12.7999592405442,-67.9633488277327,
-80.0127685614673));
#30904=CARTESIAN_POINT('Ctrl Pts',(-12.799946040306,-67.9672266123404,-80.0148361348949));
#30905=CARTESIAN_POINT('Ctrl Pts',(-12.7999280866335,-67.9715824544212,
-80.0171605578629));
#30906=CARTESIAN_POINT('Ctrl Pts',(-12.7999022340551,-67.9764781077637,
-80.0197750909363));
#30907=CARTESIAN_POINT('Ctrl Pts',(-12.7998752238266,-67.9815929830961,
-80.0225066999344));
#30908=CARTESIAN_POINT('Ctrl Pts',(-12.7998395772213,-67.9872968847195,
-80.0255548709977));
#30909=CARTESIAN_POINT('Ctrl Pts',(-12.7997907696023,-67.9936068349789,
-80.0289288405153));
#30910=CARTESIAN_POINT('Ctrl Pts',(-12.7997391599796,-68.0002790340856,
-80.032496506737));
#30911=CARTESIAN_POINT('Ctrl Pts',(-12.7996727937154,-68.0076285898944,
-80.0364283082196));
#30912=CARTESIAN_POINT('Ctrl Pts',(-12.7995857188208,-68.0156208516721,
-80.0407056886438));
#30913=CARTESIAN_POINT('Ctrl Pts',(-12.799491696128,-68.0242508244868,-80.045324365785));
#30914=CARTESIAN_POINT('Ctrl Pts',(-12.7993734425619,-68.0336297662844,
-80.0503457624994));
#30915=CARTESIAN_POINT('Ctrl Pts',(-12.7992237895711,-68.04365689647,-80.0557156998772));
#30916=CARTESIAN_POINT('Ctrl Pts',(-12.7990546437389,-68.0549900965059,
-80.0617850909547));
#30917=CARTESIAN_POINT('Ctrl Pts',(-12.7988452033844,-68.0671506433314,
-80.0682993625326));
#30918=CARTESIAN_POINT('Ctrl Pts',(-12.7985877510598,-68.0799305652783,
-80.0751465322796));
#30919=CARTESIAN_POINT('Ctrl Pts',(-12.7982019864598,-68.0990799028725,
-80.0854062792165));
#30920=CARTESIAN_POINT('Ctrl Pts',(-12.7977069522051,-68.1196165458355,
-80.0964116800166));
#30921=CARTESIAN_POINT('Ctrl Pts',(-12.7970969250991,-68.1407215549374,
-80.1077212688361));
#30922=CARTESIAN_POINT('Ctrl Pts',(-12.7966664795798,-68.1556136089336,
-80.1157015073929));
#30923=CARTESIAN_POINT('Ctrl Pts',(-12.7961794307637,-68.170784726054,-80.1238310754694));
#30924=CARTESIAN_POINT('Ctrl Pts',(-12.7956415403645,-68.1859667653999,
-80.1319653074543));
#30925=CARTESIAN_POINT('Ctrl Pts',(-12.7951858474735,-68.1988287674205,
-80.1388565100024));
#30926=CARTESIAN_POINT('Ctrl Pts',(-12.7946938680268,-68.2116980075239,
-80.1457507392318));
#30927=CARTESIAN_POINT('Ctrl Pts',(-12.7941713799325,-68.2244477542231,
-80.1525795119216));
#30928=CARTESIAN_POINT('Ctrl Pts',(-12.7936920887942,-68.2361434094446,
-80.158843712525));
#30929=CARTESIAN_POINT('Ctrl Pts',(-12.7931872421108,-68.2477381387599,
-80.1650526367671));
#30930=CARTESIAN_POINT('Ctrl Pts',(-12.7926613499875,-68.2591736887779,
-80.1711746016963));
#30931=CARTESIAN_POINT('Ctrl Pts',(-12.7921657812218,-68.2699498558987,
-80.176943569265));
#30932=CARTESIAN_POINT('Ctrl Pts',(-12.7916516116072,-68.280584401439,-80.1826351780779));
#30933=CARTESIAN_POINT('Ctrl Pts',(-12.791121256113,-68.2910697963873,-80.1882449028664));
#30934=CARTESIAN_POINT('Ctrl Pts',(-12.7906144706368,-68.3010892002192,
-80.1936053206968));
#30935=CARTESIAN_POINT('Ctrl Pts',(-12.7900929767344,-68.3109722050848,
-80.1988908644493));
#30936=CARTESIAN_POINT('Ctrl Pts',(-12.7895564864506,-68.3207544709881,
-80.2041200314091));
#30937=CARTESIAN_POINT('Ctrl Pts',(-12.7890131201761,-68.3306621124503,
-80.209416218601));
#30938=CARTESIAN_POINT('Ctrl Pts',(-12.7884544756481,-68.3404657829456,
-80.2146542462203));
#30939=CARTESIAN_POINT('Ctrl Pts',(-12.7878764039241,-68.3502537016393,
-80.2198804282375));
#30940=CARTESIAN_POINT('Ctrl Pts',(-12.7873214743126,-68.3596497777528,
-80.2248973889983));
#30941=CARTESIAN_POINT('Ctrl Pts',(-12.7867481764485,-68.3690393498493,
-80.2299076786562));
#30942=CARTESIAN_POINT('Ctrl Pts',(-12.7861507958922,-68.3785104590878,
-80.2349574769543));
#30943=CARTESIAN_POINT('Ctrl Pts',(-12.7855161529563,-68.3885723409324,
-80.2403222629086));
#30944=CARTESIAN_POINT('Ctrl Pts',(-12.7848542677531,-68.3987262854919,
-80.2457316537937));
#30945=CARTESIAN_POINT('Ctrl Pts',(-12.7841604748655,-68.4090221920418,
-80.2512114845732));
#30946=CARTESIAN_POINT('Ctrl Pts',(-12.783443890586,-68.4196563235084,-80.2568713301285));
#30947=CARTESIAN_POINT('Ctrl Pts',(-12.7826932179844,-68.4304415244009,
-80.2626061141816));
#30948=CARTESIAN_POINT('Ctrl Pts',(-12.7819064372114,-68.4413782772843,
-80.2684154878918));
#30949=CARTESIAN_POINT('Ctrl Pts',(-12.7810713820932,-68.4529860742525,
-80.2745813061431));
#30950=CARTESIAN_POINT('Ctrl Pts',(-12.780195582854,-68.464764267707,-80.2808309643622));
#30951=CARTESIAN_POINT('Ctrl Pts',(-12.7792810579711,-68.4766581401074,
-80.2871349744576));
#30952=CARTESIAN_POINT('Ctrl Pts',(-12.7782865104577,-68.489592748495,-80.2939905971776));
#30953=CARTESIAN_POINT('Ctrl Pts',(-12.7772460715996,-68.502663678638,-80.300910220902));
#30954=CARTESIAN_POINT('Ctrl Pts',(-12.7761688047953,-68.5157431144594,
-80.3078260140958));
#30955=CARTESIAN_POINT('Ctrl Pts',(-12.7749095759397,-68.5310318088981,
-80.3159099597938));
#30956=CARTESIAN_POINT('Ctrl Pts',(-12.7735998467349,-68.5463312295996,
-80.3239881482717));
#30957=CARTESIAN_POINT('Ctrl Pts',(-12.7722651862118,-68.5613715074687,
-80.3319187178466));
#30958=CARTESIAN_POINT('Ctrl Pts',(-12.7705695625273,-68.5804794760765,
-80.3419941350561));
#30959=CARTESIAN_POINT('Ctrl Pts',(-12.7688336253202,-68.5991637065053,
-80.351828272569));
#30960=CARTESIAN_POINT('Ctrl Pts',(-12.7671305061878,-68.6168183625362,
-80.3611060393086));
#30961=CARTESIAN_POINT('Ctrl Pts',(-12.7659173876994,-68.6293936364735,
-80.3677145202709));
#30962=CARTESIAN_POINT('Ctrl Pts',(-12.7647215526255,-68.6414447795618,
-80.3740398914793));
#30963=CARTESIAN_POINT('Ctrl Pts',(-12.7635718386868,-68.6527752049831,
-80.3799810973145));
#30964=CARTESIAN_POINT('Ctrl Pts',(-12.7625391111644,-68.6629527298249,
-80.3853177698337));
#30965=CARTESIAN_POINT('Ctrl Pts',(-12.7615437904396,-68.6725480871623,
-80.3903441630596));
#30966=CARTESIAN_POINT('Ctrl Pts',(-12.7606047190396,-68.6814527914176,
-80.3950052350027));
#30967=CARTESIAN_POINT('Ctrl Pts',(-12.7597276128735,-68.6897699130019,
-80.3993587430981));
#30968=CARTESIAN_POINT('Ctrl Pts',(-12.758899695334,-68.6974841057397,-80.4033933523103));
#30969=CARTESIAN_POINT('Ctrl Pts',(-12.758132336613,-68.7045455229561,-80.4070844535359));
#30970=CARTESIAN_POINT('Ctrl Pts',(-12.7574026777113,-68.7112600174806,
-80.4105942134338));
#30971=CARTESIAN_POINT('Ctrl Pts',(-12.7567278489201,-68.7173839989792,
-80.4137932423359));
#30972=CARTESIAN_POINT('Ctrl Pts',(-12.7561125500973,-68.7229157499426,
-80.4166817626821));
#30973=CARTESIAN_POINT('Ctrl Pts',(-12.7554921827953,-68.7284930683007,
-80.4195940770039));
#30974=CARTESIAN_POINT('Ctrl Pts',(-12.7549324399538,-68.7334676634599,
-80.4221903926971));
#30975=CARTESIAN_POINT('Ctrl Pts',(-12.7544314042226,-68.7378886088854,
-80.4244972157607));
#30976=CARTESIAN_POINT('Ctrl Pts',(-12.753976436878,-68.7419030646919,-80.4265919349556));
#30977=CARTESIAN_POINT('Ctrl Pts',(-12.7535698402714,-68.7454612747732,
-80.4284480915835));
#30978=CARTESIAN_POINT('Ctrl Pts',(-12.7532043752489,-68.7486430334905,
-80.430107740582));
#30979=CARTESIAN_POINT('Ctrl Pts',(-12.7528471595585,-68.7517529730657,
-80.4317299277308));
#30980=CARTESIAN_POINT('Ctrl Pts',(-12.7525292584261,-68.7545030695974,
-80.4331642771879));
#30981=CARTESIAN_POINT('Ctrl Pts',(-12.7522381260796,-68.7570112163957,
-80.4344724376543));
#30982=CARTESIAN_POINT('Ctrl Pts',(-12.7519553737875,-68.7594471678263,
-80.435742943576));
#30983=CARTESIAN_POINT('Ctrl Pts',(-12.7516978784384,-68.7616547969803,
-80.4368943675231));
#30984=CARTESIAN_POINT('Ctrl Pts',(-12.7514484579662,-68.7637855518688,
-80.4380056117235));
#30985=CARTESIAN_POINT('Ctrl Pts',(-12.7513493910281,-68.7646318631635,
-80.4384469851179));
#30986=CARTESIAN_POINT('Ctrl Pts',(-12.7512515330953,-68.7654665461706,
-80.4388822776113));
#30987=CARTESIAN_POINT('Ctrl Pts',(-12.7511535426466,-68.7663011286799,
-80.439317485445));
#30988=CARTESIAN_POINT('',(-12.7960011616543,-69.2365750327735,-79.5595260961694));
#30989=CARTESIAN_POINT('Ctrl Pts',(-12.7960011616543,-69.2365750327735,
-79.5595260961694));
#30990=CARTESIAN_POINT('Ctrl Pts',(-12.7810519553184,-69.0798170647423,
-79.8527898925946));
#30991=CARTESIAN_POINT('Ctrl Pts',(-12.7661027489825,-68.9230590967111,
-80.1460536890198));
#30992=CARTESIAN_POINT('Ctrl Pts',(-12.7511535426466,-68.7663011286799,
-80.439317485445));
#30993=CARTESIAN_POINT('',(-12.8,-69.,-79.4330532904862));
#30994=CARTESIAN_POINT('Ctrl Pts',(-12.7960011616543,-69.2365750327735,
-79.5595260961694));
#30995=CARTESIAN_POINT('Ctrl Pts',(-12.7960292083229,-69.2357456361795,
-79.5590825116583));
#30996=CARTESIAN_POINT('Ctrl Pts',(-12.7960572613955,-69.2349121483207,
-79.5586367411658));
#30997=CARTESIAN_POINT('Ctrl Pts',(-12.7960893559361,-69.2339523963487,
-79.5581234407148));
#30998=CARTESIAN_POINT('Ctrl Pts',(-12.7961226721972,-69.2329561101666,
-79.557590600813));
#30999=CARTESIAN_POINT('Ctrl Pts',(-12.7961603390279,-69.2318239510054,
-79.5569850918275));
#31000=CARTESIAN_POINT('Ctrl Pts',(-12.7962049226453,-69.2304705628775,
-79.5562612669052));
#31001=CARTESIAN_POINT('Ctrl Pts',(-12.7962515945371,-69.229053782726,-79.5555035383852));
#31002=CARTESIAN_POINT('Ctrl Pts',(-12.7963058396059,-69.2273947972326,
-79.5546162755396));
#31003=CARTESIAN_POINT('Ctrl Pts',(-12.7963685818537,-69.2254477031397,
-79.5535749397574));
#31004=CARTESIAN_POINT('Ctrl Pts',(-12.7964351401458,-69.2233821848954,
-79.5524702689228));
#31005=CARTESIAN_POINT('Ctrl Pts',(-12.7965112434551,-69.2209927570776,
-79.5511923799426));
#31006=CARTESIAN_POINT('Ctrl Pts',(-12.7965959456592,-69.218277743219,-79.5497403965593));
#31007=CARTESIAN_POINT('Ctrl Pts',(-12.7966879808357,-69.2153276809137,
-79.5481627097886));
#31008=CARTESIAN_POINT('Ctrl Pts',(-12.7967901299217,-69.2119936833039,
-79.5463797291895));
#31009=CARTESIAN_POINT('Ctrl Pts',(-12.7968992523985,-69.2083287109004,
-79.5444198073676));
#31010=CARTESIAN_POINT('Ctrl Pts',(-12.7970274017946,-69.2040247030171,
-79.5421181477523));
#31011=CARTESIAN_POINT('Ctrl Pts',(-12.7971650772674,-69.1992650434548,
-79.5395728952846));
#31012=CARTESIAN_POINT('Ctrl Pts',(-12.7973056545457,-69.1941998374416,
-79.5368643629279));
#31013=CARTESIAN_POINT('Ctrl Pts',(-12.7974945510837,-69.1873936174649,
-79.5332248531063));
#31014=CARTESIAN_POINT('Ctrl Pts',(-12.7976882456695,-69.1800418837563,
-79.5292938348712));
#31015=CARTESIAN_POINT('Ctrl Pts',(-12.7978725057253,-69.172569967302,-79.5252987931617));
#31016=CARTESIAN_POINT('Ctrl Pts',(-12.797995425483,-69.1675854569241,-79.5226337035582));
#31017=CARTESIAN_POINT('Ctrl Pts',(-12.7981142248542,-69.1625489535661,
-79.5199409172442));
#31018=CARTESIAN_POINT('Ctrl Pts',(-12.7982264691812,-69.1575635936742,
-79.5172755781975));
#31019=CARTESIAN_POINT('Ctrl Pts',(-12.7983273034916,-69.1530850125295,
-79.5148811799079));
#31020=CARTESIAN_POINT('Ctrl Pts',(-12.7984228682132,-69.1486482922782,
-79.5125092455365));
#31021=CARTESIAN_POINT('Ctrl Pts',(-12.7985126194035,-69.144295239178,-79.5101821191301));
#31022=CARTESIAN_POINT('Ctrl Pts',(-12.7985964590319,-69.1402289047641,
-79.508008271494));
#31023=CARTESIAN_POINT('Ctrl Pts',(-12.7986752428822,-69.1362359540293,
-79.5058737238968));
#31024=CARTESIAN_POINT('Ctrl Pts',(-12.7987493965746,-69.1323135818703,
-79.5037769667935));
#31025=CARTESIAN_POINT('Ctrl Pts',(-12.7988210097945,-69.1285255884331,
-79.5017520436541));
#31026=CARTESIAN_POINT('Ctrl Pts',(-12.7988883185632,-69.1248038214923,
-79.4997625802429));
#31027=CARTESIAN_POINT('Ctrl Pts',(-12.7989523299241,-69.121104431999,-79.497785123555));
#31028=CARTESIAN_POINT('Ctrl Pts',(-12.7990184396467,-69.1172837725157,
-79.4957428436974));
#31029=CARTESIAN_POINT('Ctrl Pts',(-12.7990811576708,-69.1134805580376,
-79.4937099361942));
#31030=CARTESIAN_POINT('Ctrl Pts',(-12.799141584533,-69.1096224414086,-79.4916477126436));
#31031=CARTESIAN_POINT('Ctrl Pts',(-12.7992029440752,-69.1057047753016,
-79.4895536589676));
#31032=CARTESIAN_POINT('Ctrl Pts',(-12.7992619121947,-69.101730635701,-79.4874294505204));
#31033=CARTESIAN_POINT('Ctrl Pts',(-12.7993184858065,-69.0976766822073,
-79.4852626001243));
#31034=CARTESIAN_POINT('Ctrl Pts',(-12.799379027078,-69.0933384140429,-79.4829437826772));
#31035=CARTESIAN_POINT('Ctrl Pts',(-12.7994367896057,-69.088909139761,-79.4805763439809));
#31036=CARTESIAN_POINT('Ctrl Pts',(-12.7994909980303,-69.08441426712,-79.4781738549575));
#31037=CARTESIAN_POINT('Ctrl Pts',(-12.7995513398687,-69.0794108219781,
-79.4754995362408));
#31038=CARTESIAN_POINT('Ctrl Pts',(-12.7996072226821,-69.0743267169926,
-79.4727821199101));
#31039=CARTESIAN_POINT('Ctrl Pts',(-12.799657409628,-69.0692542261559,-79.4700709151347));
#31040=CARTESIAN_POINT('Ctrl Pts',(-12.7997276364042,-69.062156271242,-79.4662771164119));
#31041=CARTESIAN_POINT('Ctrl Pts',(-12.7997864800475,-69.055082683729,-79.4624963494086));
#31042=CARTESIAN_POINT('Ctrl Pts',(-12.7998327796974,-69.0483844631479,
-79.4589161926673));
#31043=CARTESIAN_POINT('Ctrl Pts',(-12.7998710512233,-69.0428476799647,
-79.455956816905));
#31044=CARTESIAN_POINT('Ctrl Pts',(-12.7999008268853,-69.0375723115798,
-79.4531371510512));
#31045=CARTESIAN_POINT('Ctrl Pts',(-12.7999233926443,-69.0327490016854,
-79.4505590809883));
#31046=CARTESIAN_POINT('Ctrl Pts',(-12.7999421370997,-69.0287424749182,
-79.4484175833567));
#31047=CARTESIAN_POINT('Ctrl Pts',(-12.7999559634565,-69.0250487403429,
-79.4464432528478));
#31048=CARTESIAN_POINT('Ctrl Pts',(-12.7999662322845,-69.0217427430679,
-79.4446761446091));
#31049=CARTESIAN_POINT('Ctrl Pts',(-12.7999757221325,-69.0186875344802,
-79.4430430869212));
#31050=CARTESIAN_POINT('Ctrl Pts',(-12.799982198985,-69.0159640572094,-79.4415873197681));
#31051=CARTESIAN_POINT('Ctrl Pts',(-12.7999868084143,-69.0135897765305,
-79.4403181795648));
#31052=CARTESIAN_POINT('Ctrl Pts',(-12.7999909974299,-69.0114320475654,
-79.4391647942041));
#31053=CARTESIAN_POINT('Ctrl Pts',(-12.7999936526088,-69.0095627953852,
-79.4381655843713));
#31054=CARTESIAN_POINT('Ctrl Pts',(-12.7999954793624,-69.007955432479,-79.4373063421029));
#31055=CARTESIAN_POINT('Ctrl Pts',(-12.7999972411368,-69.0064052448995,
-79.4364776638455));
#31056=CARTESIAN_POINT('Ctrl Pts',(-12.799998233814,-69.0050989506826,-79.4357793352319));
#31057=CARTESIAN_POINT('Ctrl Pts',(-12.7999988737608,-69.0039708119737,
-79.4351762234692));
#31058=CARTESIAN_POINT('Ctrl Pts',(-12.7999994864525,-69.002890720218,-79.434598797983));
#31059=CARTESIAN_POINT('Ctrl Pts',(-12.7999997736227,-69.0019740761535,
-79.4341087286492));
#31060=CARTESIAN_POINT('Ctrl Pts',(-12.7999999102358,-69.0011210258309,
-79.4336526479403));
#31061=CARTESIAN_POINT('Ctrl Pts',(-12.7999999713847,-69.0007391951752,
-79.4334485033647));
#31062=CARTESIAN_POINT('Ctrl Pts',(-12.8,-69.0003695148519,-79.4332508527041));
#31063=CARTESIAN_POINT('Ctrl Pts',(-12.8,-69.,-79.4330532904862));
#31064=CARTESIAN_POINT('',(-12.8,-68.4696699141101,-79.7165266452431));
#31065=CARTESIAN_POINT('Ctrl Pts',(-6.03657703353082,-75.9960010939969,
-79.5595271661918));
#31066=CARTESIAN_POINT('Ctrl Pts',(-6.03327711009717,-75.9961126843306,
-79.5577622746215));
#31067=CARTESIAN_POINT('Ctrl Pts',(-6.02026638500826,-75.996630632865,-79.5508024334891));
#31068=CARTESIAN_POINT('Ctrl Pts',(-5.95065337319764,-75.9985039356983,
-79.5135784929313));
#31069=CARTESIAN_POINT('Ctrl Pts',(-5.8859377473749,-75.9995834393596,-79.4789880070745));
#31070=CARTESIAN_POINT('Ctrl Pts',(-5.81635363943525,-76.0000779190584,
-79.4417961750041));
#31071=CARTESIAN_POINT('Ctrl Pts',(-5.80330218536736,-76.,-79.4348188137443));
#31072=CARTESIAN_POINT('Ctrl Pts',(-5.8,-76.,-79.4330532904862));
#31073=CARTESIAN_POINT('Ctrl Pts',(-5.87981905585798,-75.9810518330436,
-79.8527909486792));
#31074=CARTESIAN_POINT('Ctrl Pts',(-5.87376087109586,-75.9813470906745,
-79.8495905670206));
#31075=CARTESIAN_POINT('Ctrl Pts',(-5.84397742479736,-75.9831739264559,
-79.8337977365213));
#31076=CARTESIAN_POINT('Ctrl Pts',(-5.72771843298234,-75.9889126186106,
-79.7718564493927));
#31077=CARTESIAN_POINT('Ctrl Pts',(-5.59861589417875,-75.9951964527643,
-79.7031094075536));
#31078=CARTESIAN_POINT('Ctrl Pts',(-5.48236810616443,-75.9992414076862,
-79.6411504971624));
#31079=CARTESIAN_POINT('Ctrl Pts',(-5.45251738072014,-76.,-79.6252655486369));
#31080=CARTESIAN_POINT('Ctrl Pts',(-5.44644660940672,-76.,-79.6220355269908));
#31081=CARTESIAN_POINT('Ctrl Pts',(-5.72306107818513,-75.9661025720903,
-80.1460547311667));
#31082=CARTESIAN_POINT('Ctrl Pts',(-5.71423060572681,-75.9668146627209,
-80.141423247653));
#31083=CARTESIAN_POINT('Ctrl Pts',(-5.68537900484321,-75.9714758414277,
-80.1262751604081));
#31084=CARTESIAN_POINT('Ctrl Pts',(-5.48880129776891,-75.9845626296476,
-80.0204498936597));
#31085=CARTESIAN_POINT('Ctrl Pts',(-5.32713079429893,-75.9958857681933,
-79.9346800344166));
#31086=CARTESIAN_POINT('Ctrl Pts',(-5.13072552883509,-75.9990090085338,
-79.8304586573348));
#31087=CARTESIAN_POINT('Ctrl Pts',(-5.10173257607291,-76.,-79.8157122835296));
#31088=CARTESIAN_POINT('Ctrl Pts',(-5.09289321881345,-76.,-79.8110177634954));
#31089=CARTESIAN_POINT('Ctrl Pts',(-5.56630310051229,-75.9511533111369,
-80.4393185136542));
#31090=CARTESIAN_POINT('Ctrl Pts',(-5.55473194650397,-75.9525119129618,
-80.4332845306404));
#31091=CARTESIAN_POINT('Ctrl Pts',(-5.50914529119826,-75.9587873887317,
-80.4097053660028));
#31092=CARTESIAN_POINT('Ctrl Pts',(-5.26592447242786,-75.9815925202367,
-80.2818324443123));
#31093=CARTESIAN_POINT('Ctrl Pts',(-5.03984373668773,-75.994897210969,-80.1608657662782));
#31094=CARTESIAN_POINT('Ctrl Pts',(-4.79674752703822,-76.0009537785116,
-80.0305411221384));
#31095=CARTESIAN_POINT('Ctrl Pts',(-4.75094777142568,-76.,-80.0061590184222));
#31096=CARTESIAN_POINT('Ctrl Pts',(-4.73933982822017,-76.,-80.));
#31097=CARTESIAN_POINT('',(-5.8,-76.,-79.4330532904862));
#31098=CARTESIAN_POINT('',(-6.03657703353082,-75.9960010939969,-79.5595271661918));
#31099=CARTESIAN_POINT('Ctrl Pts',(-5.8,-76.,-79.4330532904862));
#31100=CARTESIAN_POINT('Ctrl Pts',(-5.80082995274897,-76.,-79.4334970271994));
#31101=CARTESIAN_POINT('Ctrl Pts',(-5.80166399480472,-75.9999998681034,
-79.4339429495971));
#31102=CARTESIAN_POINT('Ctrl Pts',(-5.80262437266497,-75.9999995080477,
-79.4344563936532));
#31103=CARTESIAN_POINT('Ctrl Pts',(-5.80362130731139,-75.9999991342865,
-79.4349893819589));
#31104=CARTESIAN_POINT('Ctrl Pts',(-5.80475419180803,-75.9999985165435,
-79.4355950302349));
#31105=CARTESIAN_POINT('Ctrl Pts',(-5.80610842551985,-75.999997334795,-79.4363189799149));
#31106=CARTESIAN_POINT('Ctrl Pts',(-5.80752608820132,-75.9999960976964,
-79.4370768376138));
#31107=CARTESIAN_POINT('Ctrl Pts',(-5.80918608700224,-75.9999942436748,
-79.4379642132424));
#31108=CARTESIAN_POINT('Ctrl Pts',(-5.8111343338153,-75.9999911447523,-79.4390056428645));
#31109=CARTESIAN_POINT('Ctrl Pts',(-5.81320106845652,-75.9999878573605,
-79.4401104098078));
#31110=CARTESIAN_POINT('Ctrl Pts',(-5.81559186714737,-75.9999831623473,
-79.4413883725241));
#31111=CARTESIAN_POINT('Ctrl Pts',(-5.81830837518257,-75.9999760573446,
-79.4428404081802));
#31112=CARTESIAN_POINT('Ctrl Pts',(-5.82126004291222,-75.9999683372839,
-79.4444181420697));
#31113=CARTESIAN_POINT('Ctrl Pts',(-5.82459578581144,-75.9999577493602,
-79.4462011419664));
#31114=CARTESIAN_POINT('Ctrl Pts',(-5.8282625676441,-75.9999429445725,-79.4481610611416));
#31115=CARTESIAN_POINT('Ctrl Pts',(-5.83256856471686,-75.999925558926,-79.4504626450964));
#31116=CARTESIAN_POINT('Ctrl Pts',(-5.8373302706201,-75.9999022941867,-79.4530077763197));
#31117=CARTESIAN_POINT('Ctrl Pts',(-5.84239745159174,-75.9998716028295,
-79.455716163997));
#31118=CARTESIAN_POINT('Ctrl Pts',(-5.84920772213249,-75.9998303537706,
-79.459356225979));
#31119=CARTESIAN_POINT('Ctrl Pts',(-5.85656359157639,-75.9997754571138,
-79.4632878747617));
#31120=CARTESIAN_POINT('Ctrl Pts',(-5.86403923384336,-75.9997070636227,
-79.4672835414454));
#31121=CARTESIAN_POINT('Ctrl Pts',(-5.86902545581198,-75.9996614454515,
-79.4699486343278));
#31122=CARTESIAN_POINT('Ctrl Pts',(-5.87406347506768,-75.9996099513757,
-79.4726414127709));
#31123=CARTESIAN_POINT('Ctrl Pts',(-5.87905011371789,-75.9995536343056,
-79.4753067390642));
#31124=CARTESIAN_POINT('Ctrl Pts',(-5.88352984403094,-75.9995030420523,
-79.4777011261108));
#31125=CARTESIAN_POINT('Ctrl Pts',(-5.88796752306019,-75.9994485978456,
-79.4800730453466));
#31126=CARTESIAN_POINT('Ctrl Pts',(-5.89232133734403,-75.9993911714285,
-79.4824001558454));
#31127=CARTESIAN_POINT('Ctrl Pts',(-5.89638838293447,-75.9993375274645,
-79.4845739886907));
#31128=CARTESIAN_POINT('Ctrl Pts',(-5.90038187319399,-75.9992813110251,
-79.4867085208515));
#31129=CARTESIAN_POINT('Ctrl Pts',(-5.90430461639031,-75.9992228530745,
-79.4888052625665));
#31130=CARTESIAN_POINT('Ctrl Pts',(-5.90809297579459,-75.9991663977532,
-79.4908301749294));
#31131=CARTESIAN_POINT('Ctrl Pts',(-5.91181495196092,-75.9991078793035,
-79.4928196274862));
#31132=CARTESIAN_POINT('Ctrl Pts',(-5.91551439553953,-75.9990468225626,
-79.4947970718196));
#31133=CARTESIAN_POINT('Ctrl Pts',(-5.91933528783517,-75.9989837613951,
-79.496839433504));
#31134=CARTESIAN_POINT('Ctrl Pts',(-5.92313856760111,-75.9989179008181,
-79.4988724198909));
#31135=CARTESIAN_POINT('Ctrl Pts',(-5.92699658801122,-75.9988478956635,
-79.5009347238149));
#31136=CARTESIAN_POINT('Ctrl Pts',(-5.93091408408494,-75.9987768113019,
-79.5030288204412));
#31137=CARTESIAN_POINT('Ctrl Pts',(-5.9348878842878,-75.9987014292312,-79.5051530722866));
#31138=CARTESIAN_POINT('Ctrl Pts',(-5.93894132412967,-75.9986209576208,
-79.5073199663828));
#31139=CARTESIAN_POINT('Ctrl Pts',(-5.94327904087287,-75.9985348423544,
-79.5096388296616));
#31140=CARTESIAN_POINT('Ctrl Pts',(-5.94770756311628,-75.998442875431,-79.5120063144621));
#31141=CARTESIAN_POINT('Ctrl Pts',(-5.95220148345265,-75.9983451407054,
-79.5144088470737));
#31142=CARTESIAN_POINT('Ctrl Pts',(-5.95720386716646,-75.9982363478113,
-79.5170832135752));
#31143=CARTESIAN_POINT('Ctrl Pts',(-5.96228666106351,-75.9981203739986,
-79.5198006744923));
#31144=CARTESIAN_POINT('Ctrl Pts',(-5.96735762017057,-75.9979991016698,
-79.5225119144319));
#31145=CARTESIAN_POINT('Ctrl Pts',(-5.97445334315968,-75.9978294069763,
-79.5263057150053));
#31146=CARTESIAN_POINT('Ctrl Pts',(-5.98152426064256,-75.9976491625957,
-79.530086465422));
#31147=CARTESIAN_POINT('Ctrl Pts',(-5.98821959813878,-75.9974690698049,
-79.5336665749896));
#31148=CARTESIAN_POINT('Ctrl Pts',(-5.99375413982361,-75.9973202003778,
-79.5366259875134));
#31149=CARTESIAN_POINT('Ctrl Pts',(-5.99902711332963,-75.9971716764186,
-79.5394456619015));
#31150=CARTESIAN_POINT('Ctrl Pts',(-6.0038480455955,-75.9970312257633,-79.5420236998642));
#31151=CARTESIAN_POINT('Ctrl Pts',(-6.00785256740384,-75.9969145600064,
-79.5441651548101));
#31152=CARTESIAN_POINT('Ctrl Pts',(-6.01154431600515,-75.9968035509036,
-79.546139417071));
#31153=CARTESIAN_POINT('Ctrl Pts',(-6.01484844630879,-75.9967020906366,
-79.5479064292275));
#31154=CARTESIAN_POINT('Ctrl Pts',(-6.01790182492339,-75.9966083302274,
-79.5495393421681));
#31155=CARTESIAN_POINT('Ctrl Pts',(-6.02062359805108,-75.9965227694684,
-79.5509949530694));
#31156=CARTESIAN_POINT('Ctrl Pts',(-6.02299635741864,-75.9964471429846,
-79.5522639279905));
#31157=CARTESIAN_POINT('Ctrl Pts',(-6.02515277768795,-75.9963784118336,
-79.5534172026455));
#31158=CARTESIAN_POINT('Ctrl Pts',(-6.02702085252075,-75.9963178969774,
-79.5544162836354));
#31159=CARTESIAN_POINT('Ctrl Pts',(-6.02862718080636,-75.9962654046424,
-79.5552753829552));
#31160=CARTESIAN_POINT('Ctrl Pts',(-6.03017636954699,-75.9962147795398,
-79.556103922803));
#31161=CARTESIAN_POINT('Ctrl Pts',(-6.03148179822677,-75.9961716280755,
-79.5568021000397));
#31162=CARTESIAN_POINT('Ctrl Pts',(-6.0326091820744,-75.9961341445412,-79.5574050543401));
#31163=CARTESIAN_POINT('Ctrl Pts',(-6.03368855155447,-75.9960982574002,
-79.5579823293037));
#31164=CARTESIAN_POINT('Ctrl Pts',(-6.03460457466333,-75.9960675683623,
-79.5584722424552));
#31165=CARTESIAN_POINT('Ctrl Pts',(-6.03545705366498,-75.9960388775277,
-79.5589281707029));
#31166=CARTESIAN_POINT('Ctrl Pts',(-6.03583852510599,-75.9960260388138,
-79.559132191688));
#31167=CARTESIAN_POINT('Ctrl Pts',(-6.03620786239713,-75.9960135779017,
-79.5593297231193));
#31168=CARTESIAN_POINT('Ctrl Pts',(-6.03657703353082,-75.9960010939969,
-79.5595271661918));
#31169=CARTESIAN_POINT('',(-5.56630310051229,-75.9511533111369,-80.4393185136542));
#31170=CARTESIAN_POINT('Ctrl Pts',(-5.56630310051229,-75.9511533111369,
-80.4393185136542));
#31171=CARTESIAN_POINT('Ctrl Pts',(-5.72306107818513,-75.9661025720903,
-80.1460547311667));
#31172=CARTESIAN_POINT('Ctrl Pts',(-5.87981905585798,-75.9810518330436,
-79.8527909486792));
#31173=CARTESIAN_POINT('Ctrl Pts',(-6.03657703353082,-75.9960010939969,
-79.5595271661918));
#31174=CARTESIAN_POINT('',(-4.73933982822017,-76.,-80.));
#31175=CARTESIAN_POINT('Ctrl Pts',(-5.56630310051229,-75.9511533111369,
-80.4393185136542));
#31176=CARTESIAN_POINT('Ctrl Pts',(-5.56420681552843,-75.9513994418688,
-80.4382253687547));
#31177=CARTESIAN_POINT('Ctrl Pts',(-5.56210662013596,-75.9516451623633,
-80.4371299982174));
#31178=CARTESIAN_POINT('Ctrl Pts',(-5.55983393131473,-75.9519098993802,
-80.4359446578429));
#31179=CARTESIAN_POINT('Ctrl Pts',(-5.55750339571347,-75.952181374752,-80.4347291469833));
#31180=CARTESIAN_POINT('Ctrl Pts',(-5.55499160002995,-75.9524728344429,
-80.4334190935274));
#31181=CARTESIAN_POINT('Ctrl Pts',(-5.55216503325917,-75.9527989364359,
-80.4319448041763));
#31182=CARTESIAN_POINT('Ctrl Pts',(-5.54925619217981,-75.9531345304445,
-80.4304276019394));
#31183=CARTESIAN_POINT('Ctrl Pts',(-5.54601413463847,-75.9535068018879,
-80.428736540034));
#31184=CARTESIAN_POINT('Ctrl Pts',(-5.54234178307442,-75.9539253137786,
-80.4268206510647));
#31185=CARTESIAN_POINT('Ctrl Pts',(-5.53846827069886,-75.9543667505418,
-80.4247998152314));
#31186=CARTESIAN_POINT('Ctrl Pts',(-5.53411605254984,-75.9548596340652,
-80.4225288569658));
#31187=CARTESIAN_POINT('Ctrl Pts',(-5.52922332488371,-75.9554081743592,
-80.4199748464482));
#31188=CARTESIAN_POINT('Ctrl Pts',(-5.52411129332526,-75.9559813015565,
-80.4173063589996));
#31189=CARTESIAN_POINT('Ctrl Pts',(-5.51840942455183,-75.9566151484006,
-80.414328981764));
#31190=CARTESIAN_POINT('Ctrl Pts',(-5.51210072583542,-75.9573073476311,
-80.4110327808206));
#31191=CARTESIAN_POINT('Ctrl Pts',(-5.50542940200128,-75.9580393345958,
-80.4075471136642));
#31192=CARTESIAN_POINT('Ctrl Pts',(-5.49807975731088,-75.9588365034254,
-80.4037050492189));
#31193=CARTESIAN_POINT('Ctrl Pts',(-5.49008657713406,-75.9596890414977,
-80.399523291729));
#31194=CARTESIAN_POINT('Ctrl Pts',(-5.48145450988579,-75.9606097221039,
-80.395007290454));
#31195=CARTESIAN_POINT('Ctrl Pts',(-5.47207231574455,-75.9615948484974,
-80.39009530727));
#31196=CARTESIAN_POINT('Ctrl Pts',(-5.46204108178782,-75.962625655139,-80.3848383268206));
#31197=CARTESIAN_POINT('Ctrl Pts',(-5.45069945656391,-75.9637911172006,
-80.3788946211584));
#31198=CARTESIAN_POINT('Ctrl Pts',(-5.43852884548578,-75.9650147154232,
-80.3725102190935));
#31199=CARTESIAN_POINT('Ctrl Pts',(-5.42573797772755,-75.9662645146503,
-80.3657920972725));
#31200=CARTESIAN_POINT('Ctrl Pts',(-5.40663505197305,-75.9681310668103,
-80.3557587058889));
#31201=CARTESIAN_POINT('Ctrl Pts',(-5.38615199235454,-75.9700542679493,
-80.3449823921339));
#31202=CARTESIAN_POINT('Ctrl Pts',(-5.36510219960243,-75.9719331684186,
-80.3338855781411));
#31203=CARTESIAN_POINT('Ctrl Pts',(-5.35021359138999,-75.9732621227359,
-80.3260367542647));
#31204=CARTESIAN_POINT('Ctrl Pts',(-5.33504537194617,-75.9745690761541,
-80.3180297742239));
#31205=CARTESIAN_POINT('Ctrl Pts',(-5.31986575382764,-75.9758280745175,
-80.3100055159971));
#31206=CARTESIAN_POINT('Ctrl Pts',(-5.30700487317325,-75.9768947566678,
-80.3032069900665));
#31207=CARTESIAN_POINT('Ctrl Pts',(-5.29413641239381,-75.9779271418622,
-80.2963964149645));
#31208=CARTESIAN_POINT('Ctrl Pts',(-5.28138714940104,-75.9789158885675,
-80.2896409949838));
#31209=CARTESIAN_POINT('Ctrl Pts',(-5.26969165141048,-75.9798229123782,
-80.2834439308198));
#31210=CARTESIAN_POINT('Ctrl Pts',(-5.25809683612155,-75.9806932835307,
-80.2772934958828));
#31211=CARTESIAN_POINT('Ctrl Pts',(-5.24666095829357,-75.9815244583872,
-80.2712209815137));
#31212=CARTESIAN_POINT('Ctrl Pts',(-5.23588434009871,-75.9823077173742,
-80.2654985376555));
#31213=CARTESIAN_POINT('Ctrl Pts',(-5.22524913290962,-75.9830562233904,
-80.2598454426357));
#31214=CARTESIAN_POINT('Ctrl Pts',(-5.21476282203278,-75.9837713308532,
-80.2542662126294));
#31215=CARTESIAN_POINT('Ctrl Pts',(-5.20474245968912,-75.9844546632449,
-80.2489348900205));
#31216=CARTESIAN_POINT('Ctrl Pts',(-5.19485826674047,-75.9851075444798,
-80.2436711326451));
#31217=CARTESIAN_POINT('Ctrl Pts',(-5.18507449508653,-75.9857337373977,
-80.2384565456445));
#31218=CARTESIAN_POINT('Ctrl Pts',(-5.17521478296077,-75.9863647907505,
-80.2332014836398));
#31219=CARTESIAN_POINT('Ctrl Pts',(-5.16545763849053,-75.9869687713007,
-80.2279966720334));
#31220=CARTESIAN_POINT('Ctrl Pts',(-5.15571614445803,-75.9875516791372,
-80.2227965950344));
#31221=CARTESIAN_POINT('Ctrl Pts',(-5.14631664806357,-75.9881141226484,
-80.2177790787437));
#31222=CARTESIAN_POINT('Ctrl Pts',(-5.13692376966904,-75.9886574246325,
-80.2127617589355));
#31223=CARTESIAN_POINT('Ctrl Pts',(-5.12744922457989,-75.9891861239043,
-80.2076982534025));
#31224=CARTESIAN_POINT('Ctrl Pts',(-5.11738549871931,-75.9897477006856,
-80.2023198704724));
#31225=CARTESIAN_POINT('Ctrl Pts',(-5.10722959513758,-75.9902927448358,
-80.1968893513437));
#31226=CARTESIAN_POINT('Ctrl Pts',(-5.09693143911862,-75.9908223093185,
-80.1913805965077));
#31227=CARTESIAN_POINT('Ctrl Pts',(-5.08630134840889,-75.9913689429565,
-80.1856942810648));
#31228=CARTESIAN_POINT('Ctrl Pts',(-5.07552006464755,-75.9918989882314,
-80.1799247984738));
#31229=CARTESIAN_POINT('Ctrl Pts',(-5.06458696526359,-75.9924103020835,
-80.1740723646978));
#31230=CARTESIAN_POINT('Ctrl Pts',(-5.05298361295765,-75.992952961997,-80.1678611478631));
#31231=CARTESIAN_POINT('Ctrl Pts',(-5.04120958294207,-75.9934744148136,
-80.1615566624296));
#31232=CARTESIAN_POINT('Ctrl Pts',(-5.0293193642881,-75.9939700334766,-80.1551886129752));
#31233=CARTESIAN_POINT('Ctrl Pts',(-5.01639002675629,-75.9945089656164,
-80.148264042182));
#31234=CARTESIAN_POINT('Ctrl Pts',(-5.0033237905166,-75.9950171983507,-80.1412645651398));
#31235=CARTESIAN_POINT('Ctrl Pts',(-4.99024809552006,-75.9954885369991,
-80.1342590730832));
#31236=CARTESIAN_POINT('Ctrl Pts',(-4.97497270795401,-75.9960391678093,
-80.1260750640279));
#31237=CARTESIAN_POINT('Ctrl Pts',(-4.95968530337708,-75.9965391539293,
-80.1178833208327));
#31238=CARTESIAN_POINT('Ctrl Pts',(-4.94465465779552,-75.9969821282777,
-80.1098288638723));
#31239=CARTESIAN_POINT('Ctrl Pts',(-4.9255177507954,-75.9975461199481,-80.0995739887274));
#31240=CARTESIAN_POINT('Ctrl Pts',(-4.90680250399691,-75.9980169438008,
-80.0895446021287));
#31241=CARTESIAN_POINT('Ctrl Pts',(-4.88911665148895,-75.9983966220755,
-80.0800683512843));
#31242=CARTESIAN_POINT('Ctrl Pts',(-4.87653281631635,-75.9986667707055,
-80.0733258106786));
#31243=CARTESIAN_POINT('Ctrl Pts',(-4.86447189641292,-75.9988912194174,
-80.066864252552));
#31244=CARTESIAN_POINT('Ctrl Pts',(-4.85313058056598,-75.9990759421802,
-80.0607896158592));
#31245=CARTESIAN_POINT('Ctrl Pts',(-4.84294408761826,-75.999241855655,-80.0553335255195));
#31246=CARTESIAN_POINT('Ctrl Pts',(-4.83333877115914,-75.999375843044,-80.0501899245532));
#31247=CARTESIAN_POINT('Ctrl Pts',(-4.8244232494793,-75.9994842520891,-80.0454172395432));
#31248=CARTESIAN_POINT('Ctrl Pts',(-4.81609630495915,-75.99958550428,-80.0409596335031));
#31249=CARTESIAN_POINT('Ctrl Pts',(-4.80837149988448,-75.99966451597,-80.0368258070939));
#31250=CARTESIAN_POINT('Ctrl Pts',(-4.80129886613601,-75.9997270278736,
-80.0330426087309));
#31251=CARTESIAN_POINT('Ctrl Pts',(-4.79457383079584,-75.9997864675076,
-80.0294453430454));
#31252=CARTESIAN_POINT('Ctrl Pts',(-4.78843874020103,-75.9998310313963,
-80.0261652479022));
#31253=CARTESIAN_POINT('Ctrl Pts',(-4.78289555168418,-75.9998653972212,
-80.0232032971218));
#31254=CARTESIAN_POINT('Ctrl Pts',(-4.77729879020271,-75.9999000951797,
-80.0202127201302));
#31255=CARTESIAN_POINT('Ctrl Pts',(-4.77230613724924,-75.9999244270673,
-80.0175468458571));
#31256=CARTESIAN_POINT('Ctrl Pts',(-4.76786861194713,-75.9999423966778,
-80.0151792611979));
#31257=CARTESIAN_POINT('Ctrl Pts',(-4.76384513769839,-75.9999586896025,
-80.0130325881629));
#31258=CARTESIAN_POINT('Ctrl Pts',(-4.76027774664032,-75.9999697470085,
-80.0111309831632));
#31259=CARTESIAN_POINT('Ctrl Pts',(-4.75708692753788,-75.9999777607848,
-80.0094316682683));
#31260=CARTESIAN_POINT('Ctrl Pts',(-4.75396812364608,-75.9999855936941,
-80.007770706071));
#31261=CARTESIAN_POINT('Ctrl Pts',(-4.7512092797227,-75.9999905148514,-80.0063031091167));
#31262=CARTESIAN_POINT('Ctrl Pts',(-4.74869284463608,-75.9999938354518,
-80.0049656978208));
#31263=CARTESIAN_POINT('Ctrl Pts',(-4.74624891473313,-75.9999970603769,
-80.0036668208992));
#31264=CARTESIAN_POINT('Ctrl Pts',(-4.74403372650234,-75.9999987706602,
-80.0024907890072));
#31265=CARTESIAN_POINT('Ctrl Pts',(-4.74189623642452,-75.9999995399948,
-80.0013564736068));
#31266=CARTESIAN_POINT('Ctrl Pts',(-4.74103601494663,-75.9999998496094,
-80.0008999744256));
#31267=CARTESIAN_POINT('Ctrl Pts',(-4.74018786870459,-76.,-80.0004499588664));
#31268=CARTESIAN_POINT('Ctrl Pts',(-4.73933982822017,-76.,-80.));
#31269=CARTESIAN_POINT('',(-5.26966991411008,-76.,-79.7165266452431));
#31270=CARTESIAN_POINT('Ctrl Pts',(-5.56630310051229,-75.9511533111369,
-80.4393185136542));
#31271=CARTESIAN_POINT('Ctrl Pts',(-6.42601048595868,-75.8502126424846,
-80.8876281426549));
#31272=CARTESIAN_POINT('Ctrl Pts',(-8.03268023872916,-75.3730832556622,
-81.6648999492777));
#31273=CARTESIAN_POINT('Ctrl Pts',(-9.43111245203295,-74.4444873881411,
-82.0000000010328));
#31274=CARTESIAN_POINT('Ctrl Pts',(-9.95543453132142,-73.9999999953529,
-82.));
#31275=CARTESIAN_POINT('Ctrl Pts',(-5.72306107818513,-75.9661025720903,
-80.1460547311667));
#31276=CARTESIAN_POINT('Ctrl Pts',(-6.58258916750901,-75.8891242237522,
-80.5980971288505));
#31277=CARTESIAN_POINT('Ctrl Pts',(-8.18232324202342,-75.4545140008688,
-81.4026226152872));
#31278=CARTESIAN_POINT('Ctrl Pts',(-9.56281012582098,-74.5507989284016,
-81.7954256760992));
#31279=CARTESIAN_POINT('Ctrl Pts',(-10.0786184794921,-74.1136110332455,
-81.8224303038977));
#31280=CARTESIAN_POINT('Ctrl Pts',(-5.87981905585798,-75.9810518330436,
-79.8527909486792));
#31281=CARTESIAN_POINT('Ctrl Pts',(-6.73916784905935,-75.9280358050199,
-80.3085661150462));
#31282=CARTESIAN_POINT('Ctrl Pts',(-8.33196624531768,-75.5359447460753,
-81.1403452812968));
#31283=CARTESIAN_POINT('Ctrl Pts',(-9.69450779960901,-74.6571104686622,
-81.5908513511656));
#31284=CARTESIAN_POINT('Ctrl Pts',(-10.2018024276628,-74.2272220711382,
-81.6448606077953));
#31285=CARTESIAN_POINT('Ctrl Pts',(-6.03657703353082,-75.9960010939969,
-79.5595271661918));
#31286=CARTESIAN_POINT('Ctrl Pts',(-6.89574653060969,-75.9669473862876,
-80.0190351012419));
#31287=CARTESIAN_POINT('Ctrl Pts',(-8.48160924861194,-75.6173754912818,
-80.8780679473063));
#31288=CARTESIAN_POINT('Ctrl Pts',(-9.82620547339704,-74.7634220089227,
-81.386277026232));
#31289=CARTESIAN_POINT('Ctrl Pts',(-10.3249863758336,-74.3408331090309,
-81.467290911693));
#31290=CARTESIAN_POINT('',(-10.3249863758329,-74.3408331090314,-81.4672909116929));
#31291=CARTESIAN_POINT('Ctrl Pts',(-6.03657703353082,-75.9960010939969,
-79.5595271661918));
#31292=CARTESIAN_POINT('Ctrl Pts',(-6.89574653060969,-75.9669473862876,
-80.0190351012419));
#31293=CARTESIAN_POINT('Ctrl Pts',(-8.48160924861194,-75.6173754912818,
-80.8780679473063));
#31294=CARTESIAN_POINT('Ctrl Pts',(-9.82620547339704,-74.7634220089227,
-81.386277026232));
#31295=CARTESIAN_POINT('Ctrl Pts',(-10.3249863758336,-74.3408331090309,
-81.467290911693));
#31296=CARTESIAN_POINT('',(-10.3249863758329,-74.3408331090314,-81.4672909116929));
#31297=CARTESIAN_POINT('Ctrl Pts',(-9.95543453132142,-73.9999999953529,
-82.));
#31298=CARTESIAN_POINT('Ctrl Pts',(-9.43111245203295,-74.4444873881411,
-82.0000000010328));
#31299=CARTESIAN_POINT('Ctrl Pts',(-8.03268023872916,-75.3730832556622,
-81.6648999492777));
#31300=CARTESIAN_POINT('Ctrl Pts',(-6.42601048595868,-75.8502126424846,
-80.8876281426549));
#31301=CARTESIAN_POINT('Ctrl Pts',(-5.56630310051229,-75.9511533111369,
-80.4393185136542));
#31302=CARTESIAN_POINT('Origin',(-5.8,-69.,-81.75));
#31303=CARTESIAN_POINT('',(-10.6989794855664,-74.,-81.5));
#31304=CARTESIAN_POINT('',(-10.3490523794545,-73.6428571428571,-82.));
#31305=CARTESIAN_POINT('',(-10.8,-73.8989794855664,-81.5));
#31306=CARTESIAN_POINT('Origin',(-5.8,-69.,-81.5));
#31307=CARTESIAN_POINT('',(-10.8,-73.8989794855664,-81.5));
#31308=CARTESIAN_POINT('Ctrl Pts',(-9.95543453132077,-73.9999999953534,
-82.));
#31309=CARTESIAN_POINT('Ctrl Pts',(-10.0919662599274,-73.8842569540723,
-82.));
#31310=CARTESIAN_POINT('Ctrl Pts',(-10.2227896098978,-73.7665688864269,
-82.));
#31311=CARTESIAN_POINT('Ctrl Pts',(-10.3490523794545,-73.6428571428571,
-82.));
#31312=CARTESIAN_POINT('Ctrl Pts',(-10.0786184794915,-74.1136110332461,
-81.8224303038976));
#31313=CARTESIAN_POINT('Ctrl Pts',(-10.2129332622185,-73.9997687569007,
-81.8294622194963));
#31314=CARTESIAN_POINT('Ctrl Pts',(-10.3417444835387,-73.8833507226252,
-81.8333333333333));
#31315=CARTESIAN_POINT('Ctrl Pts',(-10.4656947481584,-73.7619047619048,
-81.8333333333333));
#31316=CARTESIAN_POINT('Ctrl Pts',(-10.2018024276622,-74.2272220711388,
-81.6448606077953));
#31317=CARTESIAN_POINT('Ctrl Pts',(-10.3339002645095,-74.1152805597292,
-81.6589244389925));
#31318=CARTESIAN_POINT('Ctrl Pts',(-10.4606993571796,-74.0001325588236,
-81.6666666666667));
#31319=CARTESIAN_POINT('Ctrl Pts',(-10.5823371168624,-73.8809523809524,
-81.6666666666667));
#31320=CARTESIAN_POINT('Ctrl Pts',(-10.3249863758329,-74.3408331090314,
-81.4672909116929));
#31321=CARTESIAN_POINT('Ctrl Pts',(-10.4548672668006,-74.2307923625576,
-81.4883866584888));
#31322=CARTESIAN_POINT('Ctrl Pts',(-10.5796542308205,-74.116914395022,-81.5));
#31323=CARTESIAN_POINT('Ctrl Pts',(-10.6989794855664,-74.,-81.5));
#31324=CARTESIAN_POINT('Ctrl Pts',(-10.3249863758329,-74.3408331090314,
-81.4672909116929));
#31325=CARTESIAN_POINT('Ctrl Pts',(-10.4548672668006,-74.2307923625576,
-81.4883866584888));
#31326=CARTESIAN_POINT('Ctrl Pts',(-10.5796542308205,-74.116914395022,-81.5));
#31327=CARTESIAN_POINT('Ctrl Pts',(-10.6989794855664,-74.,-81.5));
#31328=CARTESIAN_POINT('Ctrl Pts',(-10.7999999953529,-73.1554345313214,
-82.));
#31329=CARTESIAN_POINT('Ctrl Pts',(-11.3926501132988,-72.456338117849,-82.000000001377));
#31330=CARTESIAN_POINT('Ctrl Pts',(-12.2787469320586,-70.9951705629655,
-81.554259559704));
#31331=CARTESIAN_POINT('Ctrl Pts',(-12.6754507792991,-69.4110599090621,
-80.775538373043));
#31332=CARTESIAN_POINT('Ctrl Pts',(-12.7511535426466,-68.7663011286799,
-80.439317485445));
#31333=CARTESIAN_POINT('Ctrl Pts',(-10.9136110332455,-73.2786184794921,
-81.8224303038976));
#31334=CARTESIAN_POINT('Ctrl Pts',(-11.4965284833974,-72.5908737051733,
-81.7864241176491));
#31335=CARTESIAN_POINT('Ctrl Pts',(-12.3544673189724,-71.146729879988,-81.2853611916238));
#31336=CARTESIAN_POINT('Ctrl Pts',(-12.7083706243503,-69.5676980599057,
-80.4850818794619));
#31337=CARTESIAN_POINT('Ctrl Pts',(-12.7661027489825,-68.9230590967111,
-80.1460536890198));
#31338=CARTESIAN_POINT('Ctrl Pts',(-11.0272220711382,-73.4018024276628,
-81.6448606077953));
#31339=CARTESIAN_POINT('Ctrl Pts',(-11.6004068534961,-72.7254092924976,
-81.5728482339212));
#31340=CARTESIAN_POINT('Ctrl Pts',(-12.4301877058861,-71.2982891970106,
-81.0164628235437));
#31341=CARTESIAN_POINT('Ctrl Pts',(-12.7412904694016,-69.7243362107492,
-80.1946253858808));
#31342=CARTESIAN_POINT('Ctrl Pts',(-12.7810519553184,-69.0798170647423,
-79.8527898925946));
#31343=CARTESIAN_POINT('Ctrl Pts',(-11.1408331090309,-73.5249863758335,
-81.467290911693));
#31344=CARTESIAN_POINT('Ctrl Pts',(-11.7042852235948,-72.859944879822,-81.3592723501933));
#31345=CARTESIAN_POINT('Ctrl Pts',(-12.5059080927998,-71.4498485140331,
-80.7475644554636));
#31346=CARTESIAN_POINT('Ctrl Pts',(-12.7742103144529,-69.8809743615928,
-79.9041688922997));
#31347=CARTESIAN_POINT('Ctrl Pts',(-12.7960011616543,-69.2365750327735,
-79.5595260961694));
#31348=CARTESIAN_POINT('Ctrl Pts',(-12.7511535426466,-68.7663011286799,
-80.439317485445));
#31349=CARTESIAN_POINT('Ctrl Pts',(-12.6754507792991,-69.4110599090621,
-80.775538373043));
#31350=CARTESIAN_POINT('Ctrl Pts',(-12.2787469320586,-70.9951705629655,
-81.554259559704));
#31351=CARTESIAN_POINT('Ctrl Pts',(-11.3926501132988,-72.456338117849,-82.000000001377));
#31352=CARTESIAN_POINT('Ctrl Pts',(-10.7999999953529,-73.1554345313214,
-82.));
#31353=CARTESIAN_POINT('',(-11.1408331090314,-73.5249863758329,-81.4672909116929));
#31354=CARTESIAN_POINT('',(-10.7999999970626,-73.1554345327697,-82.));
#31355=CARTESIAN_POINT('Ctrl Pts',(-11.1408331090309,-73.5249863758335,
-81.467290911693));
#31356=CARTESIAN_POINT('Ctrl Pts',(-11.7042852235948,-72.859944879822,-81.3592723501933));
#31357=CARTESIAN_POINT('Ctrl Pts',(-12.5059080927998,-71.4498485140331,
-80.7475644554636));
#31358=CARTESIAN_POINT('Ctrl Pts',(-12.7742103144529,-69.8809743615928,
-79.9041688922997));
#31359=CARTESIAN_POINT('Ctrl Pts',(-12.7960011616543,-69.2365750327735,
-79.5595260961694));
#31360=CARTESIAN_POINT('Ctrl Pts',(-10.4428571428571,-73.5490523794545,
-82.));
#31361=CARTESIAN_POINT('Ctrl Pts',(-10.5665688864269,-73.4227896098978,
-82.));
#31362=CARTESIAN_POINT('Ctrl Pts',(-10.6842569540723,-73.2919662599274,
-82.));
#31363=CARTESIAN_POINT('Ctrl Pts',(-10.7999999953534,-73.1554345313208,
-82.));
#31364=CARTESIAN_POINT('Ctrl Pts',(-10.5619047619048,-73.6656947481584,
-81.8333333333333));
#31365=CARTESIAN_POINT('Ctrl Pts',(-10.6833507226252,-73.5417444835387,
-81.8333333333333));
#31366=CARTESIAN_POINT('Ctrl Pts',(-10.7997687569007,-73.4129332622185,
-81.8294622194963));
#31367=CARTESIAN_POINT('Ctrl Pts',(-10.9136110332461,-73.2786184794915,
-81.8224303038976));
#31368=CARTESIAN_POINT('Ctrl Pts',(-10.6809523809524,-73.7823371168624,
-81.6666666666667));
#31369=CARTESIAN_POINT('Ctrl Pts',(-10.8001325588236,-73.6606993571796,
-81.6666666666667));
#31370=CARTESIAN_POINT('Ctrl Pts',(-10.9152805597292,-73.5339002645096,
-81.6589244389925));
#31371=CARTESIAN_POINT('Ctrl Pts',(-11.0272220711387,-73.4018024276622,
-81.6448606077953));
#31372=CARTESIAN_POINT('Ctrl Pts',(-10.8,-73.8989794855664,-81.5));
#31373=CARTESIAN_POINT('Ctrl Pts',(-10.9169143950219,-73.7796542308205,
-81.5));
#31374=CARTESIAN_POINT('Ctrl Pts',(-11.0307923625576,-73.6548672668006,
-81.4883866584888));
#31375=CARTESIAN_POINT('Ctrl Pts',(-11.1408331090314,-73.5249863758329,
-81.4672909116929));
#31376=CARTESIAN_POINT('Ctrl Pts',(-10.8,-73.8989794855664,-81.5));
#31377=CARTESIAN_POINT('Ctrl Pts',(-10.9169143950219,-73.7796542308205,
-81.5));
#31378=CARTESIAN_POINT('Ctrl Pts',(-11.0307923625576,-73.6548672668006,
-81.4883866584888));
#31379=CARTESIAN_POINT('Ctrl Pts',(-11.1408331090314,-73.5249863758329,
-81.4672909116929));
#31380=CARTESIAN_POINT('Origin',(-10.8,-45.,-80.));
#31381=CARTESIAN_POINT('',(-12.8,-45.,-80.));
#31382=CARTESIAN_POINT('Origin',(-12.8,-37.,-82.));
#31383=CARTESIAN_POINT('',(-12.8,-69.,-82.));
#31384=CARTESIAN_POINT('Origin',(-5.8,-69.,-82.));
#31385=CARTESIAN_POINT('',(-5.8,-76.,-82.));
#31386=CARTESIAN_POINT('Ctrl Pts',(35.9663011250092,-75.9511535430796,-80.4393174835216));
#31387=CARTESIAN_POINT('Ctrl Pts',(35.9605155618968,-75.951832840726,-80.4363004990874));
#31388=CARTESIAN_POINT('Ctrl Pts',(35.9483735247129,-75.9531618864263,-80.4299516020054));
#31389=CARTESIAN_POINT('Ctrl Pts',(35.8779762000419,-75.9616015656904,-80.3933105617495));
#31390=CARTESIAN_POINT('Ctrl Pts',(35.666496759984,-75.9813220332306,-80.282100551774));
#31391=CARTESIAN_POINT('Ctrl Pts',(35.4392833215594,-75.9946945287765,-80.1605539331644));
#31392=CARTESIAN_POINT('Ctrl Pts',(35.227860815934,-76.0000914180091,-80.0472102326352));
#31393=CARTESIAN_POINT('Ctrl Pts',(35.1573138794837,-75.9998884043116,-80.0095380402535));
#31394=CARTESIAN_POINT('Ctrl Pts',(35.1451437858069,-76.,-80.0030795017744));
#31395=CARTESIAN_POINT('Ctrl Pts',(35.1393398282202,-76.,-80.));
#31396=CARTESIAN_POINT('Ctrl Pts',(36.1230590954891,-75.9661027492297,-80.1460536883897));
#31397=CARTESIAN_POINT('Ctrl Pts',(36.11864387275,-75.9664587837152,-80.1437379532279));
#31398=CARTESIAN_POINT('Ctrl Pts',(36.110661351646,-75.9670811329732,-80.139550689276));
#31399=CARTESIAN_POINT('Ctrl Pts',(36.0600402920247,-75.9731109920079,-80.1133005606077));
#31400=CARTESIAN_POINT('Ctrl Pts',(35.8893735775267,-75.9893831955621,-80.0237135233344));
#31401=CARTESIAN_POINT('Ctrl Pts',(35.7265703748804,-75.9981653521971,-79.936367227743));
#31402=CARTESIAN_POINT('Ctrl Pts',(35.55600244748,-76.0010836873959,-79.844739492939));
#31403=CARTESIAN_POINT('Ctrl Pts',(35.5052975502908,-75.9999947733623,-79.8176043516913));
#31404=CARTESIAN_POINT('Ctrl Pts',(35.497312883448,-76.,-79.8133650160679));
#31405=CARTESIAN_POINT('Ctrl Pts',(35.4928932188134,-76.,-79.8110177634954));
#31406=CARTESIAN_POINT('Ctrl Pts',(36.2798170659691,-75.9810519553799,-79.8527898932577));
#31407=CARTESIAN_POINT('Ctrl Pts',(36.2767879876616,-75.9811995800858,-79.8511897097783));
#31408=CARTESIAN_POINT('Ctrl Pts',(36.2691521133615,-75.9816990181399,-79.8471474635063));
#31409=CARTESIAN_POINT('Ctrl Pts',(36.2292067930656,-75.9844912662356,-79.8259370154474));
#31410=CARTESIAN_POINT('Ctrl Pts',(36.1277709673604,-75.9898782465792,-79.7719436231318));
#31411=CARTESIAN_POINT('Ctrl Pts',(35.9983571190163,-75.9966058199617,-79.7030233508242));
#31412=CARTESIAN_POINT('Ctrl Pts',(35.897057117186,-75.9989497585443,-79.6490065320793));
#31413=CARTESIAN_POINT('Ctrl Pts',(35.8571253743265,-75.9998184803151,-79.6277190302889));
#31414=CARTESIAN_POINT('Ctrl Pts',(35.849481981089,-76.,-79.6236505303614));
#31415=CARTESIAN_POINT('Ctrl Pts',(35.8464466094067,-76.,-79.6220355269908));
#31416=CARTESIAN_POINT('Ctrl Pts',(36.436575036449,-75.99600116153,-79.5595260981257));
#31417=CARTESIAN_POINT('Ctrl Pts',(36.4349250886377,-75.9960569557551,-79.5586436598408));
#31418=CARTESIAN_POINT('Ctrl Pts',(36.4314614451549,-75.9961659918624,-79.5567913237265));
#31419=CARTESIAN_POINT('Ctrl Pts',(36.411343857003,-75.9968618284237,-79.5460313716173));
#31420=CARTESIAN_POINT('Ctrl Pts',(36.3508159476629,-75.9984814424111,-79.5136656592577));
#31421=CARTESIAN_POINT('Ctrl Pts',(36.2857765860264,-75.9995667759044,-79.4789019473362));
#31422=CARTESIAN_POINT('Ctrl Pts',(36.225259512466,-76.0000073927787,-79.4465563251417));
#31423=CARTESIAN_POINT('Ctrl Pts',(36.2051143900019,-75.9999908698274,-79.4357876973486));
#31424=CARTESIAN_POINT('Ctrl Pts',(36.20165107873,-76.,-79.4339360446548));
#31425=CARTESIAN_POINT('Ctrl Pts',(36.2,-76.,-79.4330532904862));
#31426=CARTESIAN_POINT('',(35.1393398282202,-76.,-80.));
#31427=CARTESIAN_POINT('',(35.9663011250092,-75.9511535430796,-80.4393174835216));
#31428=CARTESIAN_POINT('Ctrl Pts',(35.1393398282202,-76.,-80.));
#31429=CARTESIAN_POINT('Ctrl Pts',(35.1414419654955,-76.,-80.0011153657435));
#31430=CARTESIAN_POINT('Ctrl Pts',(35.1435480069179,-75.9999991196284,-80.0022328244847));
#31431=CARTESIAN_POINT('Ctrl Pts',(35.1458263157243,-75.9999970367979,-80.003442789511));
#31432=CARTESIAN_POINT('Ctrl Pts',(35.1481625809929,-75.9999949009836,-80.0046835340753));
#31433=CARTESIAN_POINT('Ctrl Pts',(35.1506798636909,-75.9999915030359,-80.0060214842795));
#31434=CARTESIAN_POINT('Ctrl Pts',(35.1535115086618,-75.9999858311707,-80.00752828776));
#31435=CARTESIAN_POINT('Ctrl Pts',(35.1564255209815,-75.9999799943212,-80.0090789213848));
#31436=CARTESIAN_POINT('Ctrl Pts',(35.1596723045489,-75.9999717556759,-80.0108082972711));
#31437=CARTESIAN_POINT('Ctrl Pts',(35.1633488277741,-75.9999592405457,-80.0127685612257));
#31438=CARTESIAN_POINT('Ctrl Pts',(35.1672266124109,-75.9999460403082,-80.0148361345773));
#31439=CARTESIAN_POINT('Ctrl Pts',(35.1715824545328,-75.9999280866369,-80.0171605574455));
#31440=CARTESIAN_POINT('Ctrl Pts',(35.1764781079312,-75.9999022340605,-80.0197750903898));
#31441=CARTESIAN_POINT('Ctrl Pts',(35.1815929833223,-75.999875223834,-80.0225066992533));
#31442=CARTESIAN_POINT('Ctrl Pts',(35.1872968850207,-75.9998395772318,-80.02555487015));
#31443=CARTESIAN_POINT('Ctrl Pts',(35.1936068353733,-75.9997907696175,-80.0289288394651));
#31444=CARTESIAN_POINT('Ctrl Pts',(35.2002790345794,-75.9997391599997,-80.0324965054732));
#31445=CARTESIAN_POINT('Ctrl Pts',(35.2076285905081,-75.9996727937424,-80.0364283067019));
#31446=CARTESIAN_POINT('Ctrl Pts',(35.215620852427,-75.9995857188577,-80.0407056868298));
#31447=CARTESIAN_POINT('Ctrl Pts',(35.2242508253968,-75.9994916961757,-80.0453243636524));
#31448=CARTESIAN_POINT('Ctrl Pts',(35.2336297673748,-75.9993734426237,-80.0503457599988));
#31449=CARTESIAN_POINT('Ctrl Pts',(35.2436568977654,-75.9992237896525,-80.0557156969594));
#31450=CARTESIAN_POINT('Ctrl Pts',(35.2549900980435,-75.9990546438421,-80.0617850875712));
#31451=CARTESIAN_POINT('Ctrl Pts',(35.2671506451442,-75.9988452035161,-80.0682993586211));
#31452=CARTESIAN_POINT('Ctrl Pts',(35.279930567395,-75.9985877512289,-80.0751465277836));
#31453=CARTESIAN_POINT('Ctrl Pts',(35.2990799056129,-75.9982019866815,-80.0854062739348));
#31454=CARTESIAN_POINT('Ctrl Pts',(35.319616549289,-75.9977069524979,-80.0964116738339));
#31455=CARTESIAN_POINT('Ctrl Pts',(35.3407215591454,-75.9970969254858,-80.1077212616672));
#31456=CARTESIAN_POINT('Ctrl Pts',(35.3556136134491,-75.9966664800393,-80.1157014994076));
#31457=CARTESIAN_POINT('Ctrl Pts',(35.3707847308888,-75.996179431309,-80.1238310666215));
#31458=CARTESIAN_POINT('Ctrl Pts',(35.3859667705584,-75.995641541008,-80.1319652977237));
#31459=CARTESIAN_POINT('Ctrl Pts',(35.3988287728834,-75.9951858481991,-80.1388564995401));
#31460=CARTESIAN_POINT('Ctrl Pts',(35.4116980132944,-75.9946938688432,-80.1457507280235));
#31461=CARTESIAN_POINT('Ctrl Pts',(35.4244477602967,-75.9941713808468,-80.1525794999723));
#31462=CARTESIAN_POINT('Ctrl Pts',(35.4361434158036,-75.9936920897979,-80.1588436998998));
#31463=CARTESIAN_POINT('Ctrl Pts',(35.4477381454004,-75.9931872432099,-80.1650526234701));
#31464=CARTESIAN_POINT('Ctrl Pts',(35.4591736956889,-75.9926613511856,-80.1711745877489));
#31465=CARTESIAN_POINT('Ctrl Pts',(35.4699498630682,-75.9921657825131,-80.1769435547067));
#31466=CARTESIAN_POINT('Ctrl Pts',(35.480584408857,-75.9916516129949,-80.1826351629276));
#31467=CARTESIAN_POINT('Ctrl Pts',(35.4910698040367,-75.9911212575979,-80.1882448871593));
#31468=CARTESIAN_POINT('Ctrl Pts',(35.5010892080918,-75.9906144722146,-80.193605304459));
#31469=CARTESIAN_POINT('Ctrl Pts',(35.5109722131649,-75.9900929784058,-80.1988908477128));
#31470=CARTESIAN_POINT('Ctrl Pts',(35.5207544792529,-75.9895564882139,-80.2041200142221));
#31471=CARTESIAN_POINT('Ctrl Pts',(35.5306621203173,-75.9890131220645,-80.209416200645));
#31472=CARTESIAN_POINT('Ctrl Pts',(35.5404657904044,-75.9884544776616,-80.2146542275518));
#31473=CARTESIAN_POINT('Ctrl Pts',(35.5502537086536,-75.9878764060606,-80.2198804089219));
#31474=CARTESIAN_POINT('Ctrl Pts',(35.5596497849624,-75.9873214765304,-80.2248973693938));
#31475=CARTESIAN_POINT('Ctrl Pts',(35.569039357218,-75.9867481787433,-80.229907658822));
#31476=CARTESIAN_POINT('Ctrl Pts',(35.5785104665749,-75.986150798257,-80.2349574569641));
#31477=CARTESIAN_POINT('Ctrl Pts',(35.5885723484862,-75.9855161553992,-80.2403222427213));
#31478=CARTESIAN_POINT('Ctrl Pts',(35.5987262930655,-75.9848542702665,-80.2457316334919));
#31479=CARTESIAN_POINT('Ctrl Pts',(35.6090221995856,-75.984160477439,-80.2512114642467));
#31480=CARTESIAN_POINT('Ctrl Pts',(35.6196563310098,-75.9834438932224,-80.2568713097704));
#31481=CARTESIAN_POINT('Ctrl Pts',(35.6304415318069,-75.9826932206728,-80.2626060938873));
#31482=CARTESIAN_POINT('Ctrl Pts',(35.6413782845434,-75.9819064399385,-80.2684154677553));
#31483=CARTESIAN_POINT('Ctrl Pts',(35.6529860813519,-75.9810713848617,-80.2745812861723));
#31484=CARTESIAN_POINT('Ctrl Pts',(35.6647642745889,-75.9801955856489,-80.2808309446627));
#31485=CARTESIAN_POINT('Ctrl Pts',(35.676658146721,-75.9792810607757,-80.2871349551246));
#31486=CARTESIAN_POINT('Ctrl Pts',(35.6895927548063,-75.9782865132737,-80.2939905782374));
#31487=CARTESIAN_POINT('Ctrl Pts',(35.702663684587,-75.9772460744072,-80.3009102024669));
#31488=CARTESIAN_POINT('Ctrl Pts',(35.7157431200006,-75.9761688075744,-80.3078259962541));
#31489=CARTESIAN_POINT('Ctrl Pts',(35.7310318138807,-75.9749095786924,-80.3159099426023));
#31490=CARTESIAN_POINT('Ctrl Pts',(35.7463312339615,-75.9735998494339,-80.3239881318513));
#31491=CARTESIAN_POINT('Ctrl Pts',(35.7613715111823,-75.972265188833,-80.3319187022711));
#31492=CARTESIAN_POINT('Ctrl Pts',(35.7804794790594,-75.9705695650414,-80.341994120603));
#31493=CARTESIAN_POINT('Ctrl Pts',(35.7991637087092,-75.9688336276876,-80.3518282593546));
#31494=CARTESIAN_POINT('Ctrl Pts',(35.8168183639804,-75.9671305083855,-80.3611060273369));
#31495=CARTESIAN_POINT('Ctrl Pts',(35.829393637445,-75.9659173897695,-80.3677145092204));
#31496=CARTESIAN_POINT('Ctrl Pts',(35.8414447800648,-75.9647215545568,-80.3740398813488));
#31497=CARTESIAN_POINT('Ctrl Pts',(35.8527752050408,-75.9635718404772,-80.3799810880625));
#31498=CARTESIAN_POINT('Ctrl Pts',(35.8629527294715,-75.9625391128293,-80.3853177613651));
#31499=CARTESIAN_POINT('Ctrl Pts',(35.8725480864178,-75.9615437919771,-80.3903441553417));
#31500=CARTESIAN_POINT('Ctrl Pts',(35.8814527903136,-75.9606047204548,-80.3950052279786));
#31501=CARTESIAN_POINT('Ctrl Pts',(35.8897699115574,-75.9597276141749,-80.3993587367197));
#31502=CARTESIAN_POINT('Ctrl Pts',(35.897484103983,-75.9588996965257,-80.4033933465282));
#31503=CARTESIAN_POINT('Ctrl Pts',(35.904545520922,-75.9581323377042,-80.4070844482868));
#31504=CARTESIAN_POINT('Ctrl Pts',(35.9112600151807,-75.9574026787072,-80.4105942086904));
#31505=CARTESIAN_POINT('Ctrl Pts',(35.9173839964454,-75.956727849829,-80.413793238041));
#31506=CARTESIAN_POINT('Ctrl Pts',(35.9229157472091,-75.9561125509301,-80.4166817587725));
#31507=CARTESIAN_POINT('Ctrl Pts',(35.9284930653801,-75.9554921835499,-80.4195940734899));
#31508=CARTESIAN_POINT('Ctrl Pts',(35.9334676603841,-75.9549324406418,-80.4221903895128));
#31509=CARTESIAN_POINT('Ctrl Pts',(35.9378886056851,-75.9544314048567,-80.424497212841));
#31510=CARTESIAN_POINT('Ctrl Pts',(35.9419030613665,-75.9539764374647,-80.4265919322698));
#31511=CARTESIAN_POINT('Ctrl Pts',(35.9454612713508,-75.9535698408206,-80.4284480890796));
#31512=CARTESIAN_POINT('Ctrl Pts',(35.9486430299948,-75.9532043757702,-80.4301077382148));
#31513=CARTESIAN_POINT('Ctrl Pts',(35.9517529694981,-75.9528471600525,-80.431729925497));
#31514=CARTESIAN_POINT('Ctrl Pts',(35.9545030659806,-75.9525292589017,-80.4331642750445));
#31515=CARTESIAN_POINT('Ctrl Pts',(35.9570112127446,-75.9522381265433,-80.4344724355708));
#31516=CARTESIAN_POINT('Ctrl Pts',(35.9594471641416,-75.9519553742397,-80.4357429415505));
#31517=CARTESIAN_POINT('Ctrl Pts',(35.9616547932761,-75.9516978788852,-80.4368943655269));
#31518=CARTESIAN_POINT('Ctrl Pts',(35.9637855481486,-75.9514484584101,-80.4380056097459));
#31519=CARTESIAN_POINT('Ctrl Pts',(35.9646318594599,-75.9513493914681,-80.4384469831598));
#31520=CARTESIAN_POINT('Ctrl Pts',(35.9654665424835,-75.9512515335318,-80.4388822756706));
#31521=CARTESIAN_POINT('Ctrl Pts',(35.9663011250092,-75.9511535430796,-80.4393174835216));
#31522=CARTESIAN_POINT('Ctrl Pts',(36.436575036449,-75.99600116153,-79.5595260981257));
#31523=CARTESIAN_POINT('Ctrl Pts',(36.2798170659691,-75.9810519553799,-79.8527898932577));
#31524=CARTESIAN_POINT('Ctrl Pts',(36.1230590954891,-75.9661027492297,-80.1460536883897));
#31525=CARTESIAN_POINT('Ctrl Pts',(35.9663011250092,-75.9511535430796,-80.4393174835216));
#31526=CARTESIAN_POINT('',(35.6696699141101,-76.,-79.7165266452431));
#31527=CARTESIAN_POINT('Ctrl Pts',(43.196001093997,-69.2365770335277,-79.5595271661901));
#31528=CARTESIAN_POINT('Ctrl Pts',(43.1961126843307,-69.2332771100941,-79.5577622746199));
#31529=CARTESIAN_POINT('Ctrl Pts',(43.1966307615514,-69.2202659648895,-79.5508022076431));
#31530=CARTESIAN_POINT('Ctrl Pts',(43.1985041525164,-69.1506531111129,-79.5135783507796));
#31531=CARTESIAN_POINT('Ctrl Pts',(43.1995836179015,-69.0859374788893,-79.4789878616826));
#31532=CARTESIAN_POINT('Ctrl Pts',(43.2000780175813,-69.0163539017547,-79.4417963142927));
#31533=CARTESIAN_POINT('Ctrl Pts',(43.2,-69.0033021853673,-79.4348188137443));
#31534=CARTESIAN_POINT('Ctrl Pts',(43.2,-69.,-79.4330532904862));
#31535=CARTESIAN_POINT('Ctrl Pts',(43.1810518330435,-69.0798190558569,-79.8527909486787));
#31536=CARTESIAN_POINT('Ctrl Pts',(43.1813470906731,-69.0737608710949,-79.8495905670201));
#31537=CARTESIAN_POINT('Ctrl Pts',(43.1831740472488,-69.0439770045782,-79.8337975102193));
#31538=CARTESIAN_POINT('Ctrl Pts',(43.188912824146,-68.9277181707527,-79.7718563065885));
#31539=CARTESIAN_POINT('Ctrl Pts',(43.1951966216217,-68.7986156255682,-79.7031092616013));
#31540=CARTESIAN_POINT('Ctrl Pts',(43.1992415012141,-68.6823683684193,-79.6411506361618));
#31541=CARTESIAN_POINT('Ctrl Pts',(43.2,-68.6525173807201,-79.6252655486369));
#31542=CARTESIAN_POINT('Ctrl Pts',(43.2,-68.6464466094067,-79.6220355269908));
#31543=CARTESIAN_POINT('Ctrl Pts',(43.1661025720901,-68.9230610781862,-80.1460547311673));
#31544=CARTESIAN_POINT('Ctrl Pts',(43.1668146627161,-68.9142306057276,-80.1414232476533));
#31545=CARTESIAN_POINT('Ctrl Pts',(43.1714769770856,-68.8853775299869,-80.1262741492686));
#31546=CARTESIAN_POINT('Ctrl Pts',(43.1845646124003,-68.6888003693769,-80.0204490165364));
#31547=CARTESIAN_POINT('Ctrl Pts',(43.1958873942081,-68.5271298441114,-79.934679223929));
#31548=CARTESIAN_POINT('Ctrl Pts',(43.1990099699337,-68.3307264381074,-79.8304589746091));
#31549=CARTESIAN_POINT('Ctrl Pts',(43.2,-68.3017325760729,-79.8157122835296));
#31550=CARTESIAN_POINT('Ctrl Pts',(43.2,-68.2928932188134,-79.8110177634954));
#31551=CARTESIAN_POINT('Ctrl Pts',(43.1511533111366,-68.7663031005154,-80.4393185136558));
#31552=CARTESIAN_POINT('Ctrl Pts',(43.1525119129614,-68.754731946507,-80.4332845306422));
#31553=CARTESIAN_POINT('Ctrl Pts',(43.1587889406164,-68.7091438168554,-80.4097047675585));
#31554=CARTESIAN_POINT('Ctrl Pts',(43.1815951370065,-68.4659235447683,-80.2818322537777));
#31555=CARTESIAN_POINT('Ctrl Pts',(43.1948993614971,-68.2398427871283,-80.160865535625));
#31556=CARTESIAN_POINT('Ctrl Pts',(43.2009549676095,-67.9967484366342,-80.0305417453682));
#31557=CARTESIAN_POINT('Ctrl Pts',(43.2,-67.9509477714257,-80.0061590184223));
#31558=CARTESIAN_POINT('Ctrl Pts',(43.2,-67.9393398282202,-80.));
#31559=CARTESIAN_POINT('',(43.1511533111366,-68.7663031005154,-80.4393185136558));
#31560=CARTESIAN_POINT('Ctrl Pts',(43.1511533111366,-68.7663031005154,-80.4393185136558));
#31561=CARTESIAN_POINT('Ctrl Pts',(43.1661025720901,-68.9230610781862,-80.1460547311673));
#31562=CARTESIAN_POINT('Ctrl Pts',(43.1810518330435,-69.0798190558569,-79.8527909486787));
#31563=CARTESIAN_POINT('Ctrl Pts',(43.196001093997,-69.2365770335277,-79.5595271661901));
#31564=CARTESIAN_POINT('Ctrl Pts',(43.1511533111366,-68.7663031005154,-80.4393185136558));
#31565=CARTESIAN_POINT('Ctrl Pts',(43.1513994418684,-68.7642068155316,-80.4382253687564));
#31566=CARTESIAN_POINT('Ctrl Pts',(43.1516451623629,-68.7621066201391,-80.4371299982191));
#31567=CARTESIAN_POINT('Ctrl Pts',(43.1519098993798,-68.7598339313178,-80.4359446578446));
#31568=CARTESIAN_POINT('Ctrl Pts',(43.1521813747516,-68.7575033957165,-80.4347291469851));
#31569=CARTESIAN_POINT('Ctrl Pts',(43.1524728344425,-68.754991600033,-80.4334190935293));
#31570=CARTESIAN_POINT('Ctrl Pts',(43.1527989364355,-68.7521650332621,-80.4319448041782));
#31571=CARTESIAN_POINT('Ctrl Pts',(43.1531345304441,-68.7492561921827,-80.4304276019414));
#31572=CARTESIAN_POINT('Ctrl Pts',(43.1535068018875,-68.7460141346413,-80.4287365400361));
#31573=CARTESIAN_POINT('Ctrl Pts',(43.1539253137781,-68.7423417830772,-80.4268206510669));
#31574=CARTESIAN_POINT('Ctrl Pts',(43.1543667505413,-68.7384682707015,-80.4247998152338));
#31575=CARTESIAN_POINT('Ctrl Pts',(43.1548596340646,-68.7341160525523,-80.4225288569684));
#31576=CARTESIAN_POINT('Ctrl Pts',(43.1554081743586,-68.729223324886,-80.4199748464511));
#31577=CARTESIAN_POINT('Ctrl Pts',(43.1559813015558,-68.7241112933274,-80.4173063590027));
#31578=CARTESIAN_POINT('Ctrl Pts',(43.1566151483999,-68.7184094245538,-80.4143289817675));
#31579=CARTESIAN_POINT('Ctrl Pts',(43.1573073476303,-68.7121007258372,-80.4110327808245));
#31580=CARTESIAN_POINT('Ctrl Pts',(43.1580393345949,-68.7054294020028,-80.4075471136685));
#31581=CARTESIAN_POINT('Ctrl Pts',(43.1588365034245,-68.6980797573121,-80.4037050492237));
#31582=CARTESIAN_POINT('Ctrl Pts',(43.1596890414966,-68.690086577135,-80.3995232917343));
#31583=CARTESIAN_POINT('Ctrl Pts',(43.1606097221028,-68.6814545098864,-80.3950072904599));
#31584=CARTESIAN_POINT('Ctrl Pts',(43.1615948484962,-68.6720723157448,-80.3900953072764));
#31585=CARTESIAN_POINT('Ctrl Pts',(43.1626256551377,-68.6620410817876,-80.3848383268276));
#31586=CARTESIAN_POINT('Ctrl Pts',(43.1637911171991,-68.6506994565633,-80.3788946211662));
#31587=CARTESIAN_POINT('Ctrl Pts',(43.1650147154216,-68.6385288454846,-80.372510219102));
#31588=CARTESIAN_POINT('Ctrl Pts',(43.1662645146486,-68.6257379777259,-80.3657920972819));
#31589=CARTESIAN_POINT('Ctrl Pts',(43.1681310668085,-68.6066350519702,-80.3557587058991));
#31590=CARTESIAN_POINT('Ctrl Pts',(43.1700542679474,-68.5861519923503,-80.3449823921449));
#31591=CARTESIAN_POINT('Ctrl Pts',(43.1719331684166,-68.565102199597,-80.3338855781529));
#31592=CARTESIAN_POINT('Ctrl Pts',(43.1732621227338,-68.5502135913843,-80.3260367542775));
#31593=CARTESIAN_POINT('Ctrl Pts',(43.1745690761519,-68.5350453719404,-80.3180297742375));
#31594=CARTESIAN_POINT('Ctrl Pts',(43.1758280745152,-68.5198657538218,-80.3100055160115));
#31595=CARTESIAN_POINT('Ctrl Pts',(43.1768947566655,-68.5070048731671,-80.3032069900815));
#31596=CARTESIAN_POINT('Ctrl Pts',(43.1779271418599,-68.4941364123874,-80.29639641498));
#31597=CARTESIAN_POINT('Ctrl Pts',(43.1789158885652,-68.4813871493945,-80.2896409949996));
#31598=CARTESIAN_POINT('Ctrl Pts',(43.1798229123759,-68.4696916514037,-80.2834439308359));
#31599=CARTESIAN_POINT('Ctrl Pts',(43.1806932835284,-68.4580968361145,-80.2772934958992));
#31600=CARTESIAN_POINT('Ctrl Pts',(43.181524458385,-68.4466609582864,-80.2712209815302));
#31601=CARTESIAN_POINT('Ctrl Pts',(43.1823077173719,-68.4358843400914,-80.2654985376722));
#31602=CARTESIAN_POINT('Ctrl Pts',(43.1830562233882,-68.4252491329023,-80.2598454426525));
#31603=CARTESIAN_POINT('Ctrl Pts',(43.1837713308511,-68.4147628220254,-80.2542662126462));
#31604=CARTESIAN_POINT('Ctrl Pts',(43.1844546632428,-68.4047424596818,-80.2489348900373));
#31605=CARTESIAN_POINT('Ctrl Pts',(43.1851075444777,-68.3948582667332,-80.2436711326619));
#31606=CARTESIAN_POINT('Ctrl Pts',(43.1857337373957,-68.3850744950793,-80.2384565456612));
#31607=CARTESIAN_POINT('Ctrl Pts',(43.1863647907485,-68.3752147829538,-80.2332014836565));
#31608=CARTESIAN_POINT('Ctrl Pts',(43.1869687712988,-68.3654576384838,-80.22799667205));
#31609=CARTESIAN_POINT('Ctrl Pts',(43.1875516791354,-68.3557161444516,-80.2227965950508));
#31610=CARTESIAN_POINT('Ctrl Pts',(43.1881141226466,-68.3463166480572,-80.2177790787598));
#31611=CARTESIAN_POINT('Ctrl Pts',(43.1886574246308,-68.3369237696628,-80.2127617589513));
#31612=CARTESIAN_POINT('Ctrl Pts',(43.1891861239027,-68.3274492245738,-80.207698253418));
#31613=CARTESIAN_POINT('Ctrl Pts',(43.189747700684,-68.3173854987134,-80.2023198704875));
#31614=CARTESIAN_POINT('Ctrl Pts',(43.1902927448343,-68.3072295951318,-80.1968893513584));
#31615=CARTESIAN_POINT('Ctrl Pts',(43.1908223093172,-68.2969314391131,-80.1913805965219));
#31616=CARTESIAN_POINT('Ctrl Pts',(43.1913689429552,-68.2863013484035,-80.1856942810786));
#31617=CARTESIAN_POINT('Ctrl Pts',(43.1918989882302,-68.2755200646424,-80.1799247984871));
#31618=CARTESIAN_POINT('Ctrl Pts',(43.1924103020824,-68.2645869652587,-80.1740723647106));
#31619=CARTESIAN_POINT('Ctrl Pts',(43.1929529619959,-68.252983612953,-80.1678611478753));
#31620=CARTESIAN_POINT('Ctrl Pts',(43.1934744148126,-68.2412095829377,-80.1615566624412));
#31621=CARTESIAN_POINT('Ctrl Pts',(43.1939700334758,-68.229319364284,-80.1551886129862));
#31622=CARTESIAN_POINT('Ctrl Pts',(43.1945089656157,-68.2163900267524,-80.1482640421924));
#31623=CARTESIAN_POINT('Ctrl Pts',(43.19501719835,-68.203323790513,-80.1412645651496));
#31624=CARTESIAN_POINT('Ctrl Pts',(43.1954885369985,-68.1902480955167,-80.1342590730923));
#31625=CARTESIAN_POINT('Ctrl Pts',(43.1960391678088,-68.174972707951,-80.1260750640363));
#31626=CARTESIAN_POINT('Ctrl Pts',(43.1965391539288,-68.1596853033743,-80.1178833208403));
#31627=CARTESIAN_POINT('Ctrl Pts',(43.1969821282773,-68.1446546577931,-80.1098288638793));
#31628=CARTESIAN_POINT('Ctrl Pts',(43.1975461199478,-68.1255177507933,-80.0995739887334));
#31629=CARTESIAN_POINT('Ctrl Pts',(43.1980169438006,-68.1068025039952,-80.089544602134));
#31630=CARTESIAN_POINT('Ctrl Pts',(43.1983966220753,-68.0891166514876,-80.0800683512888));
#31631=CARTESIAN_POINT('Ctrl Pts',(43.1986667707054,-68.0765328163152,-80.0733258106827));
#31632=CARTESIAN_POINT('Ctrl Pts',(43.1988912194173,-68.064471896412,-80.0668642525555));
#31633=CARTESIAN_POINT('Ctrl Pts',(43.1990759421801,-68.0531305805652,-80.0607896158622));
#31634=CARTESIAN_POINT('Ctrl Pts',(43.1992418556549,-68.0429440876176,-80.0553335255222));
#31635=CARTESIAN_POINT('Ctrl Pts',(43.199375843044,-68.0333387711587,-80.0501899245556));
#31636=CARTESIAN_POINT('Ctrl Pts',(43.1994842520891,-68.0244232494789,-80.0454172395453));
#31637=CARTESIAN_POINT('Ctrl Pts',(43.19958550428,-68.0160963049589,-80.0409596335049));
#31638=CARTESIAN_POINT('Ctrl Pts',(43.19966451597,-68.0083714998843,-80.0368258070954));
#31639=CARTESIAN_POINT('Ctrl Pts',(43.1997270278736,-68.0012988661359,-80.0330426087322));
#31640=CARTESIAN_POINT('Ctrl Pts',(43.1997864675076,-67.9945738307958,-80.0294453430465));
#31641=CARTESIAN_POINT('Ctrl Pts',(43.1998310313963,-67.988438740201,-80.0261652479031));
#31642=CARTESIAN_POINT('Ctrl Pts',(43.1998653972212,-67.9828955516842,-80.0232032971225));
#31643=CARTESIAN_POINT('Ctrl Pts',(43.1999000951797,-67.9772987902027,-80.0202127201308));
#31644=CARTESIAN_POINT('Ctrl Pts',(43.1999244270673,-67.9723061372493,-80.0175468458575));
#31645=CARTESIAN_POINT('Ctrl Pts',(43.1999423966778,-67.9678686119472,-80.0151792611982));
#31646=CARTESIAN_POINT('Ctrl Pts',(43.1999586896024,-67.9638451376985,-80.0130325881632));
#31647=CARTESIAN_POINT('Ctrl Pts',(43.1999697470085,-67.9602777466404,-80.0111309831634));
#31648=CARTESIAN_POINT('Ctrl Pts',(43.1999777607848,-67.957086927538,-80.0094316682685));
#31649=CARTESIAN_POINT('Ctrl Pts',(43.1999855936941,-67.9539681236462,-80.0077707060711));
#31650=CARTESIAN_POINT('Ctrl Pts',(43.1999905148514,-67.9512092797228,-80.0063031091168));
#31651=CARTESIAN_POINT('Ctrl Pts',(43.1999938354518,-67.9486928446362,-80.0049656978208));
#31652=CARTESIAN_POINT('Ctrl Pts',(43.1999970603769,-67.9462489147332,-80.0036668208992));
#31653=CARTESIAN_POINT('Ctrl Pts',(43.1999987706602,-67.9440337265024,-80.0024907890072));
#31654=CARTESIAN_POINT('Ctrl Pts',(43.1999995399948,-67.9418962364246,-80.0013564736068));
#31655=CARTESIAN_POINT('Ctrl Pts',(43.1999998496094,-67.9410360149467,-80.0008999744257));
#31656=CARTESIAN_POINT('Ctrl Pts',(43.2,-67.9401878687046,-80.0004499588664));
#31657=CARTESIAN_POINT('Ctrl Pts',(43.2,-67.9393398282202,-80.));
#31658=CARTESIAN_POINT('Ctrl Pts',(43.1511533111366,-68.7663031005154,-80.4393185136558));
#31659=CARTESIAN_POINT('Ctrl Pts',(43.0502126432029,-69.6260104798524,-80.8876281394629));
#31660=CARTESIAN_POINT('Ctrl Pts',(42.5730796190186,-71.2326776145779,-81.6649032134517));
#31661=CARTESIAN_POINT('Ctrl Pts',(41.6444873881411,-72.631112452033,-82.0000000010328));
#31662=CARTESIAN_POINT('Ctrl Pts',(41.1999999953529,-73.1554345313214,-82.));
#31663=CARTESIAN_POINT('Ctrl Pts',(43.1661025720901,-68.9230610781862,-80.1460547311673));
#31664=CARTESIAN_POINT('Ctrl Pts',(43.0891242241624,-69.7825891654741,-80.5980971278088));
#31665=CARTESIAN_POINT('Ctrl Pts',(42.6545098059633,-71.3823204079613,-81.4026261411462));
#31666=CARTESIAN_POINT('Ctrl Pts',(41.7507989284016,-72.762810125821,-81.7954256760992));
#31667=CARTESIAN_POINT('Ctrl Pts',(41.3136110332455,-73.2786184794921,-81.8224303038976));
#31668=CARTESIAN_POINT('Ctrl Pts',(43.1810518330435,-69.0798190558569,-79.8527909486787));
#31669=CARTESIAN_POINT('Ctrl Pts',(43.1280358051219,-69.9391678510958,-80.3085661161548));
#31670=CARTESIAN_POINT('Ctrl Pts',(42.735939992908,-71.5319632013446,-81.1403490688406));
#31671=CARTESIAN_POINT('Ctrl Pts',(41.8571104686622,-72.894507799609,-81.5908513511656));
#31672=CARTESIAN_POINT('Ctrl Pts',(41.4272220711382,-73.4018024276628,-81.6448606077953));
#31673=CARTESIAN_POINT('Ctrl Pts',(43.196001093997,-69.2365770335277,-79.5595271661901));
#31674=CARTESIAN_POINT('Ctrl Pts',(43.1669473860814,-70.0957465367175,-80.0190351045006));
#31675=CARTESIAN_POINT('Ctrl Pts',(42.8173701798526,-71.6816059947279,-80.8780719965351));
#31676=CARTESIAN_POINT('Ctrl Pts',(41.9634220089227,-73.0262054733971,-81.386277026232));
#31677=CARTESIAN_POINT('Ctrl Pts',(41.5408331090309,-73.5249863758335,-81.467290911693));
#31678=CARTESIAN_POINT('',(41.5408331090314,-73.5249863758329,-81.4672909116929));
#31679=CARTESIAN_POINT('Ctrl Pts',(41.1999999953529,-73.1554345313214,-82.));
#31680=CARTESIAN_POINT('Ctrl Pts',(41.6444873881411,-72.631112452033,-82.0000000010328));
#31681=CARTESIAN_POINT('Ctrl Pts',(42.5730796190186,-71.2326776145779,-81.6649032134517));
#31682=CARTESIAN_POINT('Ctrl Pts',(43.0502126432029,-69.6260104798524,-80.8876281394629));
#31683=CARTESIAN_POINT('Ctrl Pts',(43.1511533111366,-68.7663031005154,-80.4393185136558));
#31684=CARTESIAN_POINT('Origin',(36.2,-69.,-81.75));
#31685=CARTESIAN_POINT('',(40.8428571428571,-73.5490523794545,-82.));
#31686=CARTESIAN_POINT('',(41.0989794855664,-74.,-81.5));
#31687=CARTESIAN_POINT('Ctrl Pts',(41.1999999953534,-73.1554345313208,-82.));
#31688=CARTESIAN_POINT('Ctrl Pts',(41.0842569540723,-73.2919662599274,-82.));
#31689=CARTESIAN_POINT('Ctrl Pts',(40.9665688864269,-73.4227896098978,-82.));
#31690=CARTESIAN_POINT('Ctrl Pts',(40.8428571428571,-73.5490523794545,-82.));
#31691=CARTESIAN_POINT('Ctrl Pts',(41.3136110332461,-73.2786184794915,-81.8224303038976));
#31692=CARTESIAN_POINT('Ctrl Pts',(41.1997687569007,-73.4129332622185,-81.8294622194963));
#31693=CARTESIAN_POINT('Ctrl Pts',(41.0833507226253,-73.5417444835387,-81.8333333333333));
#31694=CARTESIAN_POINT('Ctrl Pts',(40.9619047619048,-73.6656947481584,-81.8333333333333));
#31695=CARTESIAN_POINT('Ctrl Pts',(41.4272220711387,-73.4018024276622,-81.6448606077953));
#31696=CARTESIAN_POINT('Ctrl Pts',(41.3152805597292,-73.5339002645095,-81.6589244389925));
#31697=CARTESIAN_POINT('Ctrl Pts',(41.2001325588236,-73.6606993571796,-81.6666666666667));
#31698=CARTESIAN_POINT('Ctrl Pts',(41.0809523809524,-73.7823371168624,-81.6666666666667));
#31699=CARTESIAN_POINT('Ctrl Pts',(41.5408331090314,-73.5249863758329,-81.4672909116929));
#31700=CARTESIAN_POINT('Ctrl Pts',(41.4307923625576,-73.6548672668006,-81.4883866584888));
#31701=CARTESIAN_POINT('Ctrl Pts',(41.316914395022,-73.7796542308205,-81.5));
#31702=CARTESIAN_POINT('Ctrl Pts',(41.2,-73.8989794855663,-81.5));
#31703=CARTESIAN_POINT('Ctrl Pts',(40.3554345313214,-73.9999999953529,-82.));
#31704=CARTESIAN_POINT('Ctrl Pts',(39.8311122212171,-74.4444875838123,-82.0000000010328));
#31705=CARTESIAN_POINT('Ctrl Pts',(38.4326814201376,-75.3730796207261,-81.6649053966967));
#31706=CARTESIAN_POINT('Ctrl Pts',(36.8259866688679,-75.8502156818532,-80.8876157483302));
#31707=CARTESIAN_POINT('Ctrl Pts',(35.9663011250092,-75.9511535430796,-80.4393174835216));
#31708=CARTESIAN_POINT('Ctrl Pts',(40.4786184794921,-74.1136110332455,-81.8224303038976));
#31709=CARTESIAN_POINT('Ctrl Pts',(39.962809898753,-74.5507991208595,-81.7954256642113));
#31710=CARTESIAN_POINT('Ctrl Pts',(38.5823210678611,-75.454510028044,-81.4026266222993));
#31711=CARTESIAN_POINT('Ctrl Pts',(36.9825801024867,-75.8891261014565,-80.5980924988281));
#31712=CARTESIAN_POINT('Ctrl Pts',(36.1230590954891,-75.9661027492297,-80.1460536883897));
#31713=CARTESIAN_POINT('Ctrl Pts',(40.6018024276628,-74.2272220711382,-81.6448606077953));
#31714=CARTESIAN_POINT('Ctrl Pts',(40.0945075762889,-74.6571106579066,-81.5908513273897));
#31715=CARTESIAN_POINT('Ctrl Pts',(38.7319607155846,-75.5359404353619,-81.140347847902));
#31716=CARTESIAN_POINT('Ctrl Pts',(37.1391735361055,-75.9280365210599,-80.308569249326));
#31717=CARTESIAN_POINT('Ctrl Pts',(36.2798170659691,-75.9810519553799,-79.8527898932577));
#31718=CARTESIAN_POINT('Ctrl Pts',(40.7249863758336,-74.3408331090309,-81.467290911693));
#31719=CARTESIAN_POINT('Ctrl Pts',(40.2262052538249,-74.7634221949538,-81.3862769905682));
#31720=CARTESIAN_POINT('Ctrl Pts',(38.8816003633081,-75.6173708426798,-80.8780690735046));
#31721=CARTESIAN_POINT('Ctrl Pts',(37.2957669697243,-75.9669469406632,-80.0190459998239));
#31722=CARTESIAN_POINT('Ctrl Pts',(36.436575036449,-75.99600116153,-79.5595260981257));
#31723=CARTESIAN_POINT('Ctrl Pts',(35.9663011250092,-75.9511535430796,-80.4393174835216));
#31724=CARTESIAN_POINT('Ctrl Pts',(36.8259866688679,-75.8502156818532,-80.8876157483302));
#31725=CARTESIAN_POINT('Ctrl Pts',(38.4326814201376,-75.3730796207261,-81.6649053966967));
#31726=CARTESIAN_POINT('Ctrl Pts',(39.8311122212171,-74.4444875838123,-82.0000000010328));
#31727=CARTESIAN_POINT('Ctrl Pts',(40.3554345313214,-73.9999999953529,-82.));
#31728=CARTESIAN_POINT('',(40.3554345327697,-73.9999999970625,-82.));
#31729=CARTESIAN_POINT('Ctrl Pts',(40.7490523794545,-73.6428571428571,-82.));
#31730=CARTESIAN_POINT('Ctrl Pts',(40.6227896098978,-73.7665688864269,-82.));
#31731=CARTESIAN_POINT('Ctrl Pts',(40.4919662599274,-73.8842569540723,-82.));
#31732=CARTESIAN_POINT('Ctrl Pts',(40.3554345313208,-73.9999999953534,-82.));
#31733=CARTESIAN_POINT('Ctrl Pts',(40.8656947481584,-73.7619047619048,-81.8333333333333));
#31734=CARTESIAN_POINT('Ctrl Pts',(40.7417444835387,-73.8833507226252,-81.8333333333333));
#31735=CARTESIAN_POINT('Ctrl Pts',(40.6129332622185,-73.9997687569007,-81.8294622194963));
#31736=CARTESIAN_POINT('Ctrl Pts',(40.4786184794915,-74.1136110332461,-81.8224303038976));
#31737=CARTESIAN_POINT('Ctrl Pts',(40.9823371168624,-73.8809523809524,-81.6666666666667));
#31738=CARTESIAN_POINT('Ctrl Pts',(40.8606993571796,-74.0001325588236,-81.6666666666667));
#31739=CARTESIAN_POINT('Ctrl Pts',(40.7339002645096,-74.1152805597292,-81.6589244389925));
#31740=CARTESIAN_POINT('Ctrl Pts',(40.6018024276622,-74.2272220711388,-81.6448606077953));
#31741=CARTESIAN_POINT('Ctrl Pts',(41.0989794855664,-74.,-81.5));
#31742=CARTESIAN_POINT('Ctrl Pts',(40.9796542308205,-74.116914395022,-81.5));
#31743=CARTESIAN_POINT('Ctrl Pts',(40.8548672668006,-74.2307923625576,-81.4883866584888));
#31744=CARTESIAN_POINT('Ctrl Pts',(40.7249863758329,-74.3408331090314,-81.4672909116929));
#31745=CARTESIAN_POINT('Origin',(41.2,-61.,-80.));
#31746=CARTESIAN_POINT('Origin',(4.7,-74.,-80.));
#31747=CARTESIAN_POINT('',(4.7,-76.,-80.));
#31748=CARTESIAN_POINT('Origin',(-5.8,-76.,-82.));
#31749=CARTESIAN_POINT('Origin',(36.2,-69.,-60.));
#31750=CARTESIAN_POINT('',(40.7,-69.,-79.5));
#31751=CARTESIAN_POINT('',(40.7,-69.,-60.));
#31752=CARTESIAN_POINT('Origin',(36.2,-69.,-79.5));
#31753=CARTESIAN_POINT('Origin',(40.7,-37.,-60.));
#31754=CARTESIAN_POINT('',(40.7,-37.,-79.5));
#31755=CARTESIAN_POINT('',(40.7,-37.,-60.));
#31756=CARTESIAN_POINT('',(40.7,-69.,-79.5));
#31757=CARTESIAN_POINT('Origin',(36.2,-37.,-60.));
#31758=CARTESIAN_POINT('',(36.2,-32.5,-79.5));
#31759=CARTESIAN_POINT('',(36.2,-32.5,-60.));
#31760=CARTESIAN_POINT('Origin',(36.2,-37.,-79.5));
#31761=CARTESIAN_POINT('Origin',(-5.8,-32.5,-60.));
#31762=CARTESIAN_POINT('',(36.2,-32.5,-79.5));
#31763=CARTESIAN_POINT('Origin',(15.2,-53.,-79.5));
#31764=CARTESIAN_POINT('',(0.,0.,0.));
#31765=CARTESIAN_POINT('Origin',(0.12,0.,0.));
#31766=CARTESIAN_POINT('',(0.24,-1.95943487863577E-16,1.6));
#31767=CARTESIAN_POINT('Origin',(0.24,0.,0.));
#31768=CARTESIAN_POINT('',(0.,2.25335011043113E-16,1.84));
#31769=CARTESIAN_POINT('',(0.12,-2.10639249453345E-16,1.72));
#31770=CARTESIAN_POINT('Origin',(0.,0.,0.));
#31771=CARTESIAN_POINT('Origin',(0.,0.,0.));
#31772=CARTESIAN_POINT('',(5.76,1.95943487863577E-16,1.6));
#31773=CARTESIAN_POINT('Origin',(5.76,0.,0.));
#31774=CARTESIAN_POINT('',(0.,-1.95943487863577E-16,1.6));
#31775=CARTESIAN_POINT('Origin',(0.,0.,0.));
#31776=CARTESIAN_POINT('',(0.,7.74764906618282,-2.22044604925031E-15));
#31777=CARTESIAN_POINT('',(0.,6.26797976099509,4.55395386103981));
#31778=CARTESIAN_POINT('',(0.,7.38978042483906,1.10140642593496));
#31779=CARTESIAN_POINT('',(0.,6.26797976099509,-4.55395386103981));
#31780=CARTESIAN_POINT('',(0.,6.62584840233885,-3.45254743510485));
#31781=CARTESIAN_POINT('',(0.,2.39415522790368,-7.36845213036123));
#31782=CARTESIAN_POINT('',(0.,3.33106749444938,-6.68774552370588));
#31783=CARTESIAN_POINT('',(0.,-2.39415522790368,-7.36845213036123));
#31784=CARTESIAN_POINT('',(0.,-1.23606797749979,-7.36845213036123));
#31785=CARTESIAN_POINT('',(0.,-6.26797976099509,-4.55395386103981));
#31786=CARTESIAN_POINT('',(0.,-5.33106749444939,-5.23466046769516));
#31787=CARTESIAN_POINT('',(0.,-7.74764906618282,1.38777878078145E-15));
#31788=CARTESIAN_POINT('',(0.,-7.38978042483906,-1.10140642593496));
#31789=CARTESIAN_POINT('',(0.,-6.26797976099509,4.55395386103981));
#31790=CARTESIAN_POINT('',(0.,-6.62584840233885,3.45254743510485));
#31791=CARTESIAN_POINT('',(0.,-2.39415522790368,7.36845213036123));
#31792=CARTESIAN_POINT('',(0.,-3.33106749444939,6.68774552370588));
#31793=CARTESIAN_POINT('',(0.,2.39415522790368,7.36845213036123));
#31794=CARTESIAN_POINT('',(0.,1.23606797749979,7.36845213036123));
#31795=CARTESIAN_POINT('',(0.,5.33106749444939,5.23466046769516));
#31796=CARTESIAN_POINT('Origin',(5.88,0.,0.));
#31797=CARTESIAN_POINT('',(6.,-2.25335011043113E-16,1.84));
#31798=CARTESIAN_POINT('Origin',(6.,0.,0.));
#31799=CARTESIAN_POINT('',(5.88,-2.10639249453345E-16,1.72));
#31800=CARTESIAN_POINT('Origin',(6.,0.,0.));
#31801=CARTESIAN_POINT('',(6.,6.25657141382095,3.29463795232411));
#31802=CARTESIAN_POINT('',(6.,6.86524758424985,3.49240882872408));
#31803=CARTESIAN_POINT('',(6.,3.5325305503885,2.40954342245162));
#31804=CARTESIAN_POINT('',(6.,6.54630003364957,4.47402845442895));
#31805=CARTESIAN_POINT('',(6.,8.,0.));
#31806=CARTESIAN_POINT('',(6.,6.27797187634959,4.84335047888998));
#31807=CARTESIAN_POINT('',(6.,6.41213595499957,4.65868946665947));
#31808=CARTESIAN_POINT('',(6.,5.44295634824952,5.45002477159954));
#31809=CARTESIAN_POINT('',(6.,6.47213595499958,4.70228201833979));
#31810=CARTESIAN_POINT('',(6.,5.06677378678233,4.93225389519957));
#31811=CARTESIAN_POINT('',(6.,3.08933132029123,2.2105378355493));
#31812=CARTESIAN_POINT('',(6.,3.12513300028246,6.34293850070151));
#31813=CARTESIAN_POINT('',(6.,3.61054319690743,5.99026734932602));
#31814=CARTESIAN_POINT('',(6.,3.50131556174964,6.86070937710148));
#31815=CARTESIAN_POINT('',(6.,1.44158315993759,4.02573093823871));
#31816=CARTESIAN_POINT('',(6.,2.66630003364957,7.46738366981103));
#31817=CARTESIAN_POINT('',(6.,6.47213595499958,4.70228201833979));
#31818=CARTESIAN_POINT('',(6.,2.23213595499958,7.60845213036123));
#31819=CARTESIAN_POINT('',(6.,2.44921799432458,7.53791790008613));
#31820=CARTESIAN_POINT('',(6.,1.2,7.60845213036123));
#31821=CARTESIAN_POINT('',(6.,2.47213595499958,7.60845213036123));
#31822=CARTESIAN_POINT('',(6.,1.2,6.96845213036123));
#31823=CARTESIAN_POINT('',(6.,1.2,3.60422606518061));
#31824=CARTESIAN_POINT('',(6.,-1.2,6.96845213036123));
#31825=CARTESIAN_POINT('',(6.,-0.6,6.96845213036123));
#31826=CARTESIAN_POINT('',(6.,-1.2,7.60845213036123));
#31827=CARTESIAN_POINT('',(6.,-1.2,4.10422606518061));
#31828=CARTESIAN_POINT('',(6.,-2.23213595499958,7.60845213036123));
#31829=CARTESIAN_POINT('',(6.,2.47213595499958,7.60845213036123));
#31830=CARTESIAN_POINT('',(6.,-2.66630003364957,7.46738366981104));
#31831=CARTESIAN_POINT('',(6.,-2.44921799432457,7.53791790008613));
#31832=CARTESIAN_POINT('',(6.,-3.50131556174964,6.86070937710148));
#31833=CARTESIAN_POINT('',(6.,-2.47213595499958,7.60845213036123));
#31834=CARTESIAN_POINT('',(6.,-3.12513300028246,6.34293850070151));
#31835=CARTESIAN_POINT('',(6.,-1.14769053379136,3.62122244105123));
#31836=CARTESIAN_POINT('',(6.,-5.06677378678233,4.93225389519957));
#31837=CARTESIAN_POINT('',(6.,-4.58136359015736,5.28492504657506));
#31838=CARTESIAN_POINT('',(6.,-5.44295634824952,5.45002477159954));
#31839=CARTESIAN_POINT('',(6.,-3.38322394643747,2.61504633273677));
#31840=CARTESIAN_POINT('',(6.,-6.27797187634959,4.84335047888998));
#31841=CARTESIAN_POINT('',(6.,-2.47213595499958,7.60845213036123));
#31842=CARTESIAN_POINT('',(6.,-6.54630003364956,4.47402845442895));
#31843=CARTESIAN_POINT('',(6.,-6.41213595499956,4.65868946665949));
#31844=CARTESIAN_POINT('',(6.,-6.86524758424985,3.49240882872408));
#31845=CARTESIAN_POINT('',(6.,-6.47213595499958,4.70228201833979));
#31846=CARTESIAN_POINT('',(6.,-6.25657141382095,3.29463795232411));
#31847=CARTESIAN_POINT('',(6.,-3.05700229224093,2.25503492526414));
#31848=CARTESIAN_POINT('',(6.,-6.99821220032083,1.01210231321574));
#31849=CARTESIAN_POINT('',(6.,-6.81280200369586,1.58273622299283));
#31850=CARTESIAN_POINT('',(6.,-7.60688837074973,1.20987318961571));
#31851=CARTESIAN_POINT('',(6.,-4.27417133688838,0.127007783343246));
#31852=CARTESIAN_POINT('',(6.,-7.92583592135001,0.228253563910838));
#31853=CARTESIAN_POINT('',(6.,-6.47213595499958,4.70228201833979));
#31854=CARTESIAN_POINT('',(6.,-7.92583592135001,-0.228253563910836));
#31855=CARTESIAN_POINT('',(6.,-7.92583592135001,4.68375338513738E-16));
#31856=CARTESIAN_POINT('',(6.,-7.60688837074973,-1.20987318961571));
#31857=CARTESIAN_POINT('',(6.,-8.,9.79717439317883E-16));
#31858=CARTESIAN_POINT('',(6.,-6.99821220032083,-1.01210231321574));
#31859=CARTESIAN_POINT('',(6.,-3.7986430787408,0.0275007138442283));
#31860=CARTESIAN_POINT('',(6.,-6.25657141382095,-3.29463795232411));
#31861=CARTESIAN_POINT('',(6.,-6.44198161044592,-2.72400404254702));
#31862=CARTESIAN_POINT('',(6.,-6.86524758424985,-3.49240882872408));
#31863=CARTESIAN_POINT('',(6.,-3.5325305503885,-2.40954342245161));
#31864=CARTESIAN_POINT('',(6.,-6.54630003364957,-4.47402845442895));
#31865=CARTESIAN_POINT('',(6.,-8.,9.79717439317883E-16));
#31866=CARTESIAN_POINT('',(6.,-6.27797187634959,-4.84335047888998));
#31867=CARTESIAN_POINT('',(6.,-6.41213595499957,-4.65868946665947));
#31868=CARTESIAN_POINT('',(6.,-5.44295634824952,-5.45002477159954));
#31869=CARTESIAN_POINT('',(6.,-6.47213595499958,-4.70228201833978));
#31870=CARTESIAN_POINT('',(6.,-5.06677378678233,-4.93225389519957));
#31871=CARTESIAN_POINT('',(6.,-3.08933132029123,-2.2105378355493));
#31872=CARTESIAN_POINT('',(6.,-3.12513300028246,-6.34293850070151));
#31873=CARTESIAN_POINT('',(6.,-3.61054319690743,-5.99026734932603));
#31874=CARTESIAN_POINT('',(6.,-3.50131556174964,-6.86070937710148));
#31875=CARTESIAN_POINT('',(6.,-1.44158315993759,-4.02573093823871));
#31876=CARTESIAN_POINT('',(6.,-2.66630003364957,-7.46738366981103));
#31877=CARTESIAN_POINT('',(6.,-6.47213595499958,-4.70228201833978));
#31878=CARTESIAN_POINT('',(6.,-2.23213595499958,-7.60845213036123));
#31879=CARTESIAN_POINT('',(6.,-2.44921799432457,-7.53791790008613));
#31880=CARTESIAN_POINT('',(6.,-1.2,-7.60845213036123));
#31881=CARTESIAN_POINT('',(6.,-2.47213595499958,-7.60845213036123));
#31882=CARTESIAN_POINT('',(6.,-1.2,-6.96845213036123));
#31883=CARTESIAN_POINT('',(6.,-1.2,-3.60422606518061));
#31884=CARTESIAN_POINT('',(6.,1.2,-6.96845213036123));
#31885=CARTESIAN_POINT('',(6.,0.6,-6.96845213036123));
#31886=CARTESIAN_POINT('',(6.,1.2,-7.60845213036123));
#31887=CARTESIAN_POINT('',(6.,1.2,-4.10422606518061));
#31888=CARTESIAN_POINT('',(6.,2.23213595499958,-7.60845213036123));
#31889=CARTESIAN_POINT('',(6.,-2.47213595499958,-7.60845213036123));
#31890=CARTESIAN_POINT('',(6.,2.66630003364957,-7.46738366981103));
#31891=CARTESIAN_POINT('',(6.,2.44921799432458,-7.53791790008613));
#31892=CARTESIAN_POINT('',(6.,3.50131556174964,-6.86070937710148));
#31893=CARTESIAN_POINT('',(6.,2.47213595499958,-7.60845213036123));
#31894=CARTESIAN_POINT('',(6.,3.12513300028246,-6.34293850070151));
#31895=CARTESIAN_POINT('',(6.,1.14769053379136,-3.62122244105123));
#31896=CARTESIAN_POINT('',(6.,5.06677378678233,-4.93225389519957));
#31897=CARTESIAN_POINT('',(6.,4.58136359015736,-5.28492504657506));
#31898=CARTESIAN_POINT('',(6.,5.44295634824952,-5.45002477159954));
#31899=CARTESIAN_POINT('',(6.,3.38322394643747,-2.61504633273677));
#31900=CARTESIAN_POINT('',(6.,6.27797187634959,-4.84335047888998));
#31901=CARTESIAN_POINT('',(6.,2.47213595499958,-7.60845213036123));
#31902=CARTESIAN_POINT('',(6.,6.54630003364957,-4.47402845442895));
#31903=CARTESIAN_POINT('',(6.,6.41213595499958,-4.65868946665946));
#31904=CARTESIAN_POINT('',(6.,6.86524758424985,-3.49240882872408));
#31905=CARTESIAN_POINT('',(6.,6.47213595499958,-4.70228201833979));
#31906=CARTESIAN_POINT('',(6.,6.25657141382095,-3.29463795232411));
#31907=CARTESIAN_POINT('',(6.,3.05700229224093,-2.25503492526414));
#31908=CARTESIAN_POINT('',(6.,6.99821220032083,-1.01210231321574));
#31909=CARTESIAN_POINT('',(6.,6.81280200369586,-1.58273622299284));
#31910=CARTESIAN_POINT('',(6.,7.60688837074973,-1.20987318961571));
#31911=CARTESIAN_POINT('',(6.,4.27417133688838,-0.127007783343246));
#31912=CARTESIAN_POINT('',(6.,7.92583592135001,-0.228253563910837));
#31913=CARTESIAN_POINT('',(6.,6.47213595499958,-4.70228201833979));
#31914=CARTESIAN_POINT('',(6.,7.92583592135001,0.228253563910837));
#31915=CARTESIAN_POINT('',(6.,7.92583592135001,6.93889390390723E-17));
#31916=CARTESIAN_POINT('',(6.,7.60688837074973,1.20987318961571));
#31917=CARTESIAN_POINT('',(6.,8.,0.));
#31918=CARTESIAN_POINT('',(6.,6.99821220032083,1.01210231321574));
#31919=CARTESIAN_POINT('',(6.,3.7986430787408,-0.0275007138442279));
#31920=CARTESIAN_POINT('',(6.,6.44198161044592,2.72400404254702));
#31921=CARTESIAN_POINT('Origin',(5.88,6.55610839240134,2.76108608187201));
#31922=CARTESIAN_POINT('',(5.76,7.22646576423166,1.08626639186573));
#31923=CARTESIAN_POINT('',(5.13,7.82563136949761,1.28094709832195));
#31924=CARTESIAN_POINT('',(5.76,6.48482497773179,3.3688020309741));
#31925=CARTESIAN_POINT('',(5.76,6.67023517435676,2.79816812119701));
#31926=CARTESIAN_POINT('',(4.88,7.32175471207153,3.64073698602405));
#31927=CARTESIAN_POINT('Origin',(3.,6.48482497773179,3.3688020309741));
#31928=CARTESIAN_POINT('',(3.,7.22646576423166,1.08626639186573));
#31929=CARTESIAN_POINT('',(3.,7.22646576423166,1.08626639186573));
#31930=CARTESIAN_POINT('',(3.,6.48482497773179,3.3688020309741));
#31931=CARTESIAN_POINT('',(3.,7.22646576423166,1.08626639186573));
#31932=CARTESIAN_POINT('',(3.,6.48482497773179,3.3688020309741));
#31933=CARTESIAN_POINT('Origin',(5.88,3.68107742718252,6.08734938865102));
#31934=CARTESIAN_POINT('',(5.76,5.20784224733253,5.12641797384956));
#31935=CARTESIAN_POINT('',(5.13,5.57814695627679,5.63609868030578));
#31936=CARTESIAN_POINT('',(5.76,3.26620146083265,6.53710257935149));
#31937=CARTESIAN_POINT('',(5.76,3.75161165745762,6.18443142797601));
#31938=CARTESIAN_POINT('',(4.88,3.78345248285003,7.24903753440145));
#31939=CARTESIAN_POINT('Origin',(3.,3.26620146083265,6.53710257935149));
#31940=CARTESIAN_POINT('',(3.,5.20784224733253,5.12641797384956));
#31941=CARTESIAN_POINT('',(3.,5.20784224733253,5.12641797384956));
#31942=CARTESIAN_POINT('',(3.,3.26620146083265,6.53710257935149));
#31943=CARTESIAN_POINT('',(3.,5.20784224733253,5.12641797384956));
#31944=CARTESIAN_POINT('',(3.,3.26620146083265,6.53710257935149));
#31945=CARTESIAN_POINT('Origin',(5.88,-0.6,7.08845213036123));
#31946=CARTESIAN_POINT('',(5.76,1.2,7.20845213036123));
#31947=CARTESIAN_POINT('',(5.13,1.2,7.83845213036123));
#31948=CARTESIAN_POINT('',(5.76,-1.2,7.20845213036123));
#31949=CARTESIAN_POINT('',(5.76,-0.6,7.20845213036123));
#31950=CARTESIAN_POINT('',(4.88,-1.2,8.08845213036123));
#31951=CARTESIAN_POINT('Origin',(3.,-1.2,7.20845213036123));
#31952=CARTESIAN_POINT('',(3.,1.2,7.20845213036123));
#31953=CARTESIAN_POINT('',(3.,1.2,7.20845213036123));
#31954=CARTESIAN_POINT('',(3.,-1.2,7.20845213036123));
#31955=CARTESIAN_POINT('',(3.,1.2,7.20845213036123));
#31956=CARTESIAN_POINT('',(3.,-1.2,7.20845213036123));
#31957=CARTESIAN_POINT('Origin',(0.,6.26797976099509,4.55395386103981));
#31958=CARTESIAN_POINT('',(0.24,6.54630003364957,4.47402845442895));
#31959=CARTESIAN_POINT('',(0.24,6.27797187634959,4.84335047888998));
#31960=CARTESIAN_POINT('',(0.24,6.54630003364957,4.47402845442895));
#31961=CARTESIAN_POINT('',(0.,6.26797976099509,4.55395386103981));
#31962=CARTESIAN_POINT('',(0.24,6.27797187634959,4.84335047888998));
#31963=CARTESIAN_POINT('Origin',(0.12,7.50390720679448,1.13848846525995));
#31964=CARTESIAN_POINT('',(0.169465769724903,7.92583592135001,-2.15105711021124E-15));
#31965=CARTESIAN_POINT('',(-0.25546881451245,7.47903325825204,-7.21644966006352E-15));
#31966=CARTESIAN_POINT('',(0.24,7.92583592135001,0.228253563910837));
#31967=CARTESIAN_POINT('',(0.24,7.61803398874989,1.17557050458495));
#31968=CARTESIAN_POINT('',(0.320496691051312,7.92583592135001,0.488746328116681));
#31969=CARTESIAN_POINT('Origin',(0.,2.39415522790368,7.36845213036123));
#31970=CARTESIAN_POINT('',(0.24,2.66630003364957,7.46738366981103));
#31971=CARTESIAN_POINT('',(0.24,2.23213595499958,7.60845213036123));
#31972=CARTESIAN_POINT('',(0.24,2.66630003364957,7.46738366981103));
#31973=CARTESIAN_POINT('',(0.,2.39415522790368,7.36845213036123));
#31974=CARTESIAN_POINT('',(0.24,2.23213595499958,7.60845213036123));
#31975=CARTESIAN_POINT('Origin',(0.12,5.40160172472448,5.33174250702015));
#31976=CARTESIAN_POINT('',(0.24,5.47213595499958,5.42882454634515));
#31977=CARTESIAN_POINT('Origin',(0.,-2.39415522790368,7.36845213036123));
#31978=CARTESIAN_POINT('',(0.24,-2.23213595499958,7.60845213036123));
#31979=CARTESIAN_POINT('',(0.24,-2.66630003364957,7.46738366981104));
#31980=CARTESIAN_POINT('',(0.24,-2.23213595499958,7.60845213036123));
#31981=CARTESIAN_POINT('',(0.,-2.39415522790368,7.36845213036123));
#31982=CARTESIAN_POINT('',(0.24,-2.66630003364957,7.46738366981104));
#31983=CARTESIAN_POINT('Origin',(0.12,1.23606797749979,7.48845213036123));
#31984=CARTESIAN_POINT('',(0.24,1.23606797749979,7.60845213036123));
#31985=CARTESIAN_POINT('Origin',(0.12,-3.40160172472448,6.78482756303088));
#31986=CARTESIAN_POINT('',(0.169465769724903,-6.41213595499958,4.65868946665946));
#31987=CARTESIAN_POINT('',(0.24,-6.27797187634959,4.84335047888998));
#31988=CARTESIAN_POINT('',(0.652102425162462,-5.49410648268598,5.92224863481158));
#31989=CARTESIAN_POINT('',(0.24,-3.47213595499958,6.88190960235587));
#31990=CARTESIAN_POINT('',(-0.255468814512445,-6.05066500742134,4.39606545060548));
#31991=CARTESIAN_POINT('Origin',(0.,-2.44921799432457,7.53791790008613));
#31992=CARTESIAN_POINT('',(0.,-2.23213595499958,7.60845213036123));
#31993=CARTESIAN_POINT('',(0.,-2.66630003364957,7.46738366981104));
#31994=CARTESIAN_POINT('Origin',(0.,2.44921799432457,7.53791790008613));
#31995=CARTESIAN_POINT('',(0.,2.66630003364957,7.46738366981103));
#31996=CARTESIAN_POINT('',(0.,2.23213595499958,7.60845213036123));
#31997=CARTESIAN_POINT('Origin',(0.,6.41213595499958,4.65868946665946));
#31998=CARTESIAN_POINT('',(0.,6.54630003364957,4.47402845442895));
#31999=CARTESIAN_POINT('',(0.,6.27797187634959,4.84335047888998));
#32000=CARTESIAN_POINT('Origin',(0.,6.47213595499958,4.70228201833979));
#32001=CARTESIAN_POINT('',(3.,3.50131556174964,6.86070937710148));
#32002=CARTESIAN_POINT('',(1.5,3.50131556174964,6.86070937710148));
#32003=CARTESIAN_POINT('',(3.,5.44295634824952,5.45002477159954));
#32004=CARTESIAN_POINT('',(3.,5.47213595499958,5.42882454634515));
#32005=CARTESIAN_POINT('',(1.5,5.44295634824952,5.45002477159954));
#32006=CARTESIAN_POINT('Origin',(0.,2.47213595499958,7.60845213036123));
#32007=CARTESIAN_POINT('',(3.,-1.2,7.60845213036123));
#32008=CARTESIAN_POINT('',(1.5,-1.2,7.60845213036123));
#32009=CARTESIAN_POINT('',(3.,1.2,7.60845213036123));
#32010=CARTESIAN_POINT('',(3.,1.23606797749979,7.60845213036123));
#32011=CARTESIAN_POINT('',(1.5,1.2,7.60845213036123));
#32012=CARTESIAN_POINT('Origin',(0.,-2.47213595499958,7.60845213036123));
#32013=CARTESIAN_POINT('',(0.,-6.27797187634959,4.84335047888998));
#32014=CARTESIAN_POINT('',(3.,-5.44295634824952,5.45002477159954));
#32015=CARTESIAN_POINT('',(1.5,-5.44295634824952,5.45002477159954));
#32016=CARTESIAN_POINT('',(3.,-3.50131556174964,6.86070937710148));
#32017=CARTESIAN_POINT('',(3.,-3.47213595499958,6.88190960235587));
#32018=CARTESIAN_POINT('',(1.5,-3.50131556174964,6.86070937710148));
#32019=CARTESIAN_POINT('Origin',(0.,-6.41213595499958,4.65868946665947));
#32020=CARTESIAN_POINT('',(0.24,-6.54630003364956,4.47402845442895));
#32021=CARTESIAN_POINT('',(0.24,-6.54630003364956,4.47402845442895));
#32022=CARTESIAN_POINT('',(0.,-6.54630003364956,4.47402845442895));
#32023=CARTESIAN_POINT('Origin',(0.12,-6.73997518429427,3.48962947442985));
#32024=CARTESIAN_POINT('',(0.24,-7.92583592135001,0.228253563910837));
#32025=CARTESIAN_POINT('',(0.,-7.74764906618282,1.66533453693773E-15));
#32026=CARTESIAN_POINT('',(0.24,-6.85410196624968,3.52671151375484));
#32027=CARTESIAN_POINT('Origin',(5.88,-4.65189782043246,5.38200708590005));
#32028=CARTESIAN_POINT('',(5.76,-3.26620146083265,6.5371025793515));
#32029=CARTESIAN_POINT('',(5.13,-3.63650616977691,7.04678328580771));
#32030=CARTESIAN_POINT('',(5.76,-5.20784224733253,5.12641797384956));
#32031=CARTESIAN_POINT('',(5.76,-4.72243205070756,5.47908912522504));
#32032=CARTESIAN_POINT('',(4.88,-5.7250932693499,5.83835292889952));
#32033=CARTESIAN_POINT('Origin',(3.,-5.20784224733253,5.12641797384956));
#32034=CARTESIAN_POINT('',(3.,-3.26620146083265,6.5371025793515));
#32035=CARTESIAN_POINT('',(3.,-3.26620146083265,6.5371025793515));
#32036=CARTESIAN_POINT('',(3.,-5.20784224733253,5.12641797384956));
#32037=CARTESIAN_POINT('',(3.,-3.26620146083265,6.5371025793515));
#32038=CARTESIAN_POINT('',(3.,-5.20784224733253,5.12641797384956));
#32039=CARTESIAN_POINT('Origin',(5.88,-6.92692878565128,1.61981826231783));
#32040=CARTESIAN_POINT('',(5.76,-6.48482497773179,3.3688020309741));
#32041=CARTESIAN_POINT('',(5.13,-7.08399058299774,3.56348273743032));
#32042=CARTESIAN_POINT('',(5.76,-7.22646576423166,1.08626639186573));
#32043=CARTESIAN_POINT('',(5.76,-7.0410555676067,1.65690030164282));
#32044=CARTESIAN_POINT('',(4.88,-8.0633954985714,1.35820134691568));
#32045=CARTESIAN_POINT('Origin',(3.,-7.22646576423166,1.08626639186573));
#32046=CARTESIAN_POINT('',(3.,-6.48482497773179,3.3688020309741));
#32047=CARTESIAN_POINT('',(3.,-6.48482497773179,3.3688020309741));
#32048=CARTESIAN_POINT('',(3.,-7.22646576423166,1.08626639186573));
#32049=CARTESIAN_POINT('',(3.,-6.48482497773179,3.3688020309741));
#32050=CARTESIAN_POINT('',(3.,-7.22646576423166,1.08626639186573));
#32051=CARTESIAN_POINT('Origin',(5.88,-6.55610839240134,-2.76108608187201));
#32052=CARTESIAN_POINT('',(5.76,-7.22646576423166,-1.08626639186573));
#32053=CARTESIAN_POINT('',(5.13,-7.82563136949761,-1.28094709832194));
#32054=CARTESIAN_POINT('',(5.76,-6.48482497773179,-3.3688020309741));
#32055=CARTESIAN_POINT('',(5.76,-6.67023517435676,-2.79816812119701));
#32056=CARTESIAN_POINT('',(4.88,-7.32175471207152,-3.64073698602405));
#32057=CARTESIAN_POINT('Origin',(3.,-6.48482497773179,-3.3688020309741));
#32058=CARTESIAN_POINT('',(3.,-7.22646576423166,-1.08626639186573));
#32059=CARTESIAN_POINT('',(3.,-7.22646576423166,-1.08626639186573));
#32060=CARTESIAN_POINT('',(3.,-6.48482497773179,-3.3688020309741));
#32061=CARTESIAN_POINT('',(3.,-7.22646576423166,-1.08626639186573));
#32062=CARTESIAN_POINT('',(3.,-6.48482497773179,-3.3688020309741));
#32063=CARTESIAN_POINT('Origin',(5.88,-3.68107742718253,-6.08734938865102));
#32064=CARTESIAN_POINT('',(5.76,-5.20784224733253,-5.12641797384956));
#32065=CARTESIAN_POINT('',(5.13,-5.57814695627679,-5.63609868030578));
#32066=CARTESIAN_POINT('',(5.76,-3.26620146083265,-6.53710257935149));
#32067=CARTESIAN_POINT('',(5.76,-3.75161165745762,-6.18443142797601));
#32068=CARTESIAN_POINT('',(4.88,-3.78345248285003,-7.24903753440145));
#32069=CARTESIAN_POINT('Origin',(3.,-3.26620146083265,-6.53710257935149));
#32070=CARTESIAN_POINT('',(3.,-5.20784224733253,-5.12641797384956));
#32071=CARTESIAN_POINT('',(3.,-5.20784224733253,-5.12641797384956));
#32072=CARTESIAN_POINT('',(3.,-3.26620146083265,-6.53710257935149));
#32073=CARTESIAN_POINT('',(3.,-5.20784224733253,-5.12641797384956));
#32074=CARTESIAN_POINT('',(3.,-3.26620146083265,-6.53710257935149));
#32075=CARTESIAN_POINT('Origin',(5.88,0.6,-7.08845213036123));
#32076=CARTESIAN_POINT('',(5.76,-1.2,-7.20845213036123));
#32077=CARTESIAN_POINT('',(5.13,-1.2,-7.83845213036123));
#32078=CARTESIAN_POINT('',(5.76,1.2,-7.20845213036123));
#32079=CARTESIAN_POINT('',(5.76,0.6,-7.20845213036123));
#32080=CARTESIAN_POINT('',(4.88,1.2,-8.08845213036123));
#32081=CARTESIAN_POINT('Origin',(3.,1.2,-7.20845213036123));
#32082=CARTESIAN_POINT('',(3.,-1.2,-7.20845213036123));
#32083=CARTESIAN_POINT('',(3.,-1.2,-7.20845213036123));
#32084=CARTESIAN_POINT('',(3.,1.2,-7.20845213036123));
#32085=CARTESIAN_POINT('',(3.,-1.2,-7.20845213036123));
#32086=CARTESIAN_POINT('',(3.,1.2,-7.20845213036123));
#32087=CARTESIAN_POINT('Origin',(5.88,4.65189782043246,-5.38200708590005));
#32088=CARTESIAN_POINT('',(5.76,3.26620146083265,-6.5371025793515));
#32089=CARTESIAN_POINT('',(5.13,3.63650616977691,-7.04678328580771));
#32090=CARTESIAN_POINT('',(5.76,5.20784224733253,-5.12641797384956));
#32091=CARTESIAN_POINT('',(5.76,4.72243205070756,-5.47908912522504));
#32092=CARTESIAN_POINT('',(4.88,5.7250932693499,-5.83835292889952));
#32093=CARTESIAN_POINT('Origin',(3.,5.20784224733253,-5.12641797384956));
#32094=CARTESIAN_POINT('',(3.,3.26620146083265,-6.5371025793515));
#32095=CARTESIAN_POINT('',(3.,3.26620146083265,-6.5371025793515));
#32096=CARTESIAN_POINT('',(3.,5.20784224733253,-5.12641797384956));
#32097=CARTESIAN_POINT('',(3.,3.26620146083265,-6.5371025793515));
#32098=CARTESIAN_POINT('',(3.,5.20784224733253,-5.12641797384956));
#32099=CARTESIAN_POINT('Origin',(0.,-7.74764906618282,1.66533453693773E-15));
#32100=CARTESIAN_POINT('',(0.24,-7.92583592135001,-0.228253563910836));
#32101=CARTESIAN_POINT('',(0.24,-7.92583592135001,0.228253563910838));
#32102=CARTESIAN_POINT('',(0.24,-7.92583592135001,-0.228253563910836));
#32103=CARTESIAN_POINT('Origin',(0.,-6.26797976099509,-4.55395386103981));
#32104=CARTESIAN_POINT('',(0.24,-6.54630003364957,-4.47402845442895));
#32105=CARTESIAN_POINT('',(0.24,-6.27797187634959,-4.84335047888998));
#32106=CARTESIAN_POINT('',(0.24,-6.54630003364957,-4.47402845442895));
#32107=CARTESIAN_POINT('',(0.,-6.26797976099509,-4.55395386103981));
#32108=CARTESIAN_POINT('',(0.24,-6.27797187634959,-4.84335047888998));
#32109=CARTESIAN_POINT('Origin',(0.12,-7.50390720679448,-1.13848846525995));
#32110=CARTESIAN_POINT('',(0.24,-7.61803398874989,-1.17557050458495));
#32111=CARTESIAN_POINT('Origin',(0.,-2.39415522790368,-7.36845213036123));
#32112=CARTESIAN_POINT('',(0.24,-2.66630003364957,-7.46738366981104));
#32113=CARTESIAN_POINT('',(0.24,-2.23213595499958,-7.60845213036123));
#32114=CARTESIAN_POINT('',(0.24,-2.66630003364957,-7.46738366981103));
#32115=CARTESIAN_POINT('',(0.,-2.39415522790368,-7.36845213036123));
#32116=CARTESIAN_POINT('',(0.24,-2.23213595499958,-7.60845213036123));
#32117=CARTESIAN_POINT('Origin',(0.12,-5.40160172472448,-5.33174250702015));
#32118=CARTESIAN_POINT('',(0.24,-5.47213595499958,-5.42882454634514));
#32119=CARTESIAN_POINT('Origin',(0.,2.39415522790368,-7.36845213036123));
#32120=CARTESIAN_POINT('',(0.24,2.23213595499958,-7.60845213036123));
#32121=CARTESIAN_POINT('',(0.24,2.66630003364957,-7.46738366981103));
#32122=CARTESIAN_POINT('',(0.24,2.23213595499958,-7.60845213036123));
#32123=CARTESIAN_POINT('',(0.,2.39415522790368,-7.36845213036123));
#32124=CARTESIAN_POINT('',(0.24,2.66630003364957,-7.46738366981103));
#32125=CARTESIAN_POINT('Origin',(0.12,-1.23606797749979,-7.48845213036123));
#32126=CARTESIAN_POINT('',(0.24,-1.23606797749979,-7.60845213036123));
#32127=CARTESIAN_POINT('Origin',(0.24,6.54630003364957,-4.47402845442895));
#32128=CARTESIAN_POINT('',(0.24,6.27797187634959,-4.84335047888998));
#32129=CARTESIAN_POINT('',(0.,6.26797976099509,-4.55395386103981));
#32130=CARTESIAN_POINT('',(0.24,6.54630003364957,-4.47402845442895));
#32131=CARTESIAN_POINT('',(0.24,6.54630003364957,-4.47402845442895));
#32132=CARTESIAN_POINT('',(0.24,6.27797187634959,-4.84335047888998));
#32133=CARTESIAN_POINT('Origin',(0.12,6.73997518429427,-3.48962947442985));
#32134=CARTESIAN_POINT('',(0.24,7.92583592135001,-0.228253563910837));
#32135=CARTESIAN_POINT('',(0.0989315394498051,7.92583592135001,0.228253563910837));
#32136=CARTESIAN_POINT('',(0.24,6.85410196624968,-3.52671151375484));
#32137=CARTESIAN_POINT('Origin',(0.,6.41213595499958,-4.65868946665946));
#32138=CARTESIAN_POINT('',(0.,6.27797187634959,-4.84335047888998));
#32139=CARTESIAN_POINT('',(0.,6.54630003364957,-4.47402845442895));
#32140=CARTESIAN_POINT('Origin',(0.12,3.40160172472448,-6.78482756303088));
#32141=CARTESIAN_POINT('',(0.24,3.47213595499958,-6.88190960235587));
#32142=CARTESIAN_POINT('Origin',(0.,7.92583592135001,1.38777878078145E-16));
#32143=CARTESIAN_POINT('',(0.,7.92583592135001,0.228253563910837));
#32144=CARTESIAN_POINT('',(0.,7.92583592135001,-0.228253563910837));
#32145=CARTESIAN_POINT('Origin',(0.,2.44921799432457,-7.53791790008613));
#32146=CARTESIAN_POINT('',(0.,2.23213595499958,-7.60845213036123));
#32147=CARTESIAN_POINT('',(0.,2.66630003364957,-7.46738366981103));
#32148=CARTESIAN_POINT('Origin',(0.,-2.44921799432457,-7.53791790008613));
#32149=CARTESIAN_POINT('',(0.,-2.66630003364957,-7.46738366981103));
#32150=CARTESIAN_POINT('',(0.,-2.23213595499958,-7.60845213036123));
#32151=CARTESIAN_POINT('Origin',(0.,-6.41213595499958,-4.65868946665946));
#32152=CARTESIAN_POINT('',(0.,-6.54630003364957,-4.47402845442895));
#32153=CARTESIAN_POINT('',(0.,-6.27797187634959,-4.84335047888998));
#32154=CARTESIAN_POINT('Origin',(0.,-7.92583592135001,9.36750677027476E-16));
#32155=CARTESIAN_POINT('',(0.,-7.92583592135001,0.228253563910838));
#32156=CARTESIAN_POINT('',(0.,-7.92583592135001,-0.228253563910836));
#32157=CARTESIAN_POINT('Origin',(0.,-6.47213595499958,4.70228201833979));
#32158=CARTESIAN_POINT('',(3.,-7.60688837074973,1.20987318961571));
#32159=CARTESIAN_POINT('',(1.5,-7.60688837074973,1.20987318961571));
#32160=CARTESIAN_POINT('',(3.,-6.86524758424985,3.49240882872408));
#32161=CARTESIAN_POINT('',(3.,-6.85410196624968,3.52671151375484));
#32162=CARTESIAN_POINT('',(1.5,-6.86524758424985,3.49240882872408));
#32163=CARTESIAN_POINT('Origin',(0.,-8.,9.79717439317883E-16));
#32164=CARTESIAN_POINT('',(3.,-6.86524758424985,-3.49240882872408));
#32165=CARTESIAN_POINT('',(1.5,-6.86524758424985,-3.49240882872408));
#32166=CARTESIAN_POINT('',(3.,-7.60688837074973,-1.20987318961571));
#32167=CARTESIAN_POINT('',(3.,-7.61803398874989,-1.17557050458495));
#32168=CARTESIAN_POINT('',(1.5,-7.60688837074973,-1.20987318961571));
#32169=CARTESIAN_POINT('Origin',(0.,-6.47213595499958,-4.70228201833978));
#32170=CARTESIAN_POINT('',(3.,-3.50131556174964,-6.86070937710147));
#32171=CARTESIAN_POINT('',(1.5,-3.50131556174964,-6.86070937710147));
#32172=CARTESIAN_POINT('',(3.,-5.44295634824952,-5.45002477159954));
#32173=CARTESIAN_POINT('',(3.,-5.47213595499958,-5.42882454634515));
#32174=CARTESIAN_POINT('',(1.5,-5.44295634824952,-5.45002477159954));
#32175=CARTESIAN_POINT('Origin',(0.,-2.47213595499958,-7.60845213036123));
#32176=CARTESIAN_POINT('',(3.,1.2,-7.60845213036123));
#32177=CARTESIAN_POINT('',(1.5,1.2,-7.60845213036123));
#32178=CARTESIAN_POINT('',(3.,-1.2,-7.60845213036123));
#32179=CARTESIAN_POINT('',(3.,-1.23606797749979,-7.60845213036123));
#32180=CARTESIAN_POINT('',(1.5,-1.2,-7.60845213036123));
#32181=CARTESIAN_POINT('Origin',(0.,2.47213595499958,-7.60845213036123));
#32182=CARTESIAN_POINT('',(3.,5.44295634824952,-5.45002477159954));
#32183=CARTESIAN_POINT('',(1.5,5.44295634824952,-5.45002477159954));
#32184=CARTESIAN_POINT('',(3.,3.50131556174964,-6.86070937710148));
#32185=CARTESIAN_POINT('',(3.,3.47213595499958,-6.88190960235587));
#32186=CARTESIAN_POINT('',(1.5,3.50131556174964,-6.86070937710148));
#32187=CARTESIAN_POINT('Origin',(5.88,6.92692878565128,-1.61981826231783));
#32188=CARTESIAN_POINT('',(5.76,6.48482497773179,-3.3688020309741));
#32189=CARTESIAN_POINT('',(5.13,7.08399058299774,-3.56348273743032));
#32190=CARTESIAN_POINT('',(5.76,7.22646576423166,-1.08626639186573));
#32191=CARTESIAN_POINT('',(5.76,7.0410555676067,-1.65690030164282));
#32192=CARTESIAN_POINT('',(4.88,8.0633954985714,-1.35820134691568));
#32193=CARTESIAN_POINT('Origin',(3.,7.22646576423166,-1.08626639186573));
#32194=CARTESIAN_POINT('',(3.,6.48482497773179,-3.3688020309741));
#32195=CARTESIAN_POINT('',(3.,6.48482497773179,-3.3688020309741));
#32196=CARTESIAN_POINT('',(3.,7.22646576423166,-1.08626639186573));
#32197=CARTESIAN_POINT('',(3.,6.48482497773179,-3.3688020309741));
#32198=CARTESIAN_POINT('',(3.,7.22646576423166,-1.08626639186573));
#32199=CARTESIAN_POINT('Origin',(3.,7.3311736291293,-2.38204270860739));
#32200=CARTESIAN_POINT('',(3.,7.60688837074973,-1.20987318961571));
#32201=CARTESIAN_POINT('',(3.,6.86524758424985,-3.49240882872408));
#32202=CARTESIAN_POINT('',(3.,6.85410196624968,-3.52671151375484));
#32203=CARTESIAN_POINT('',(3.,7.22646576423166,-1.08626639186573));
#32204=CARTESIAN_POINT('',(3.,7.43588149402694,-3.67781902534905));
#32205=CARTESIAN_POINT('Origin',(3.,6.48482497773179,-3.3688020309741));
#32206=CARTESIAN_POINT('',(1.5,6.86524758424985,-3.49240882872408));
#32207=CARTESIAN_POINT('Origin',(3.,8.17752228052682,-1.39528338624068));
#32208=CARTESIAN_POINT('',(1.5,7.60688837074973,-1.20987318961571));
#32209=CARTESIAN_POINT('Origin',(0.,6.47213595499958,-4.70228201833979));
#32210=CARTESIAN_POINT('Origin',(3.,4.53091448022882,-6.236268773788));
#32211=CARTESIAN_POINT('',(3.,5.20784224733253,-5.12641797384956));
#32212=CARTESIAN_POINT('',(3.,3.85398671312512,-7.34611957372644));
#32213=CARTESIAN_POINT('Origin',(3.,3.26620146083265,-6.5371025793515));
#32214=CARTESIAN_POINT('Origin',(3.,5.795627499625,-5.93543496822451));
#32215=CARTESIAN_POINT('Origin',(3.,-1.38777878078145E-15,-7.70845213036123));
#32216=CARTESIAN_POINT('',(3.,1.2,-7.20845213036123));
#32217=CARTESIAN_POINT('',(3.,-1.2,-8.20845213036123));
#32218=CARTESIAN_POINT('Origin',(3.,-1.2,-7.20845213036123));
#32219=CARTESIAN_POINT('Origin',(3.,1.2,-8.20845213036123));
#32220=CARTESIAN_POINT('Origin',(3.,-4.53091448022883,-6.236268773788));
#32221=CARTESIAN_POINT('',(3.,-3.26620146083265,-6.53710257935149));
#32222=CARTESIAN_POINT('',(3.,-5.795627499625,-5.93543496822451));
#32223=CARTESIAN_POINT('Origin',(3.,-5.20784224733253,-5.12641797384956));
#32224=CARTESIAN_POINT('Origin',(3.,-3.85398671312513,-7.34611957372644));
#32225=CARTESIAN_POINT('Origin',(3.,-7.3311736291293,-2.38204270860739));
#32226=CARTESIAN_POINT('',(3.,-6.48482497773179,-3.3688020309741));
#32227=CARTESIAN_POINT('',(3.,-8.17752228052682,-1.39528338624068));
#32228=CARTESIAN_POINT('Origin',(3.,-7.22646576423166,-1.08626639186573));
#32229=CARTESIAN_POINT('Origin',(3.,-7.43588149402694,-3.67781902534904));
#32230=CARTESIAN_POINT('Origin',(3.,-7.3311736291293,2.38204270860739));
#32231=CARTESIAN_POINT('',(3.,-7.22646576423166,1.08626639186573));
#32232=CARTESIAN_POINT('',(3.,-7.43588149402694,3.67781902534905));
#32233=CARTESIAN_POINT('Origin',(3.,-6.48482497773179,3.3688020309741));
#32234=CARTESIAN_POINT('Origin',(3.,-8.17752228052682,1.39528338624068));
#32235=CARTESIAN_POINT('Origin',(3.,-4.53091448022883,6.236268773788));
#32236=CARTESIAN_POINT('',(3.,-5.20784224733253,5.12641797384956));
#32237=CARTESIAN_POINT('',(3.,-3.85398671312513,7.34611957372644));
#32238=CARTESIAN_POINT('Origin',(3.,-3.26620146083265,6.5371025793515));
#32239=CARTESIAN_POINT('Origin',(3.,-5.795627499625,5.93543496822451));
#32240=CARTESIAN_POINT('Origin',(3.,5.55111512312578E-16,7.70845213036123));
#32241=CARTESIAN_POINT('',(3.,-1.2,7.20845213036123));
#32242=CARTESIAN_POINT('',(3.,1.2,8.20845213036123));
#32243=CARTESIAN_POINT('Origin',(3.,1.2,7.20845213036123));
#32244=CARTESIAN_POINT('Origin',(3.,-1.2,8.20845213036123));
#32245=CARTESIAN_POINT('Origin',(3.,4.53091448022883,6.236268773788));
#32246=CARTESIAN_POINT('',(3.,3.26620146083265,6.53710257935149));
#32247=CARTESIAN_POINT('',(3.,5.795627499625,5.93543496822451));
#32248=CARTESIAN_POINT('Origin',(3.,5.20784224733253,5.12641797384956));
#32249=CARTESIAN_POINT('Origin',(3.,3.85398671312513,7.34611957372644));
#32250=CARTESIAN_POINT('Origin',(3.,7.22646576423166,1.08626639186573));
#32251=CARTESIAN_POINT('',(3.,7.60688837074973,1.20987318961571));
#32252=CARTESIAN_POINT('',(1.5,7.60688837074973,1.20987318961571));
#32253=CARTESIAN_POINT('',(3.,8.17752228052682,1.39528338624068));
#32254=CARTESIAN_POINT('Origin',(3.,7.43588149402694,3.67781902534904));
#32255=CARTESIAN_POINT('',(3.,6.86524758424985,3.49240882872408));
#32256=CARTESIAN_POINT('',(1.5,6.86524758424985,3.49240882872408));
#32257=CARTESIAN_POINT('',(3.,6.48482497773179,3.3688020309741));
#32258=CARTESIAN_POINT('Origin',(3.,7.3311736291293,2.38204270860739));
#32259=CARTESIAN_POINT('',(3.,7.61803398874989,1.17557050458495));
#32260=CARTESIAN_POINT('Origin',(0.,8.,0.));
#32261=CARTESIAN_POINT('',(0.,0.,0.));
#32262=CARTESIAN_POINT('',(0.,0.,0.));
#32263=CARTESIAN_POINT('',(0.,0.,0.));
#32264=CARTESIAN_POINT('',(30.4,31.75,-31.75));
#32265=CARTESIAN_POINT('',(0.,0.,0.));
#32266=CARTESIAN_POINT('',(0.,0.,0.));
#32267=CARTESIAN_POINT('',(0.,0.,0.));
#32268=CARTESIAN_POINT('',(30.4,31.75,-31.75));
#32269=CARTESIAN_POINT('',(15.2,31.75,-51.65));
#32270=CARTESIAN_POINT('',(34.7,31.75,-92.75));
#32271=CARTESIAN_POINT('',(15.2,48.25,-47.75));
#32272=CARTESIAN_POINT('',(30.4,31.75,-31.75));
#32273=CARTESIAN_POINT('',(30.4,31.75,-31.75));
#32274=CARTESIAN_POINT('',(33.2,31.75,-92.75));
#32275=CARTESIAN_POINT('',(23.2,31.75,-92.75));
#32276=CARTESIAN_POINT('',(13.2,31.75,-92.75));
#32277=CARTESIAN_POINT('',(3.2,31.75,-92.75));
#32278=UNCERTAINTY_MEASURE_WITH_UNIT(LENGTH_MEASURE(0.01),#32310,
'DISTANCE_ACCURACY_VALUE',
'Maximum model space distance between geometric entities at asserted c
onnectivities');
#32279=UNCERTAINTY_MEASURE_WITH_UNIT(LENGTH_MEASURE(0.01),#32310,
'DISTANCE_ACCURACY_VALUE',
'Maximum model space distance between geometric entities at asserted c
onnectivities');
#32280=UNCERTAINTY_MEASURE_WITH_UNIT(LENGTH_MEASURE(0.01),#32310,
'DISTANCE_ACCURACY_VALUE',
'Maximum model space distance between geometric entities at asserted c
onnectivities');
#32281=UNCERTAINTY_MEASURE_WITH_UNIT(LENGTH_MEASURE(0.01),#32310,
'DISTANCE_ACCURACY_VALUE',
'Maximum model space distance between geometric entities at asserted c
onnectivities');
#32282=UNCERTAINTY_MEASURE_WITH_UNIT(LENGTH_MEASURE(0.01),#32310,
'DISTANCE_ACCURACY_VALUE',
'Maximum model space distance between geometric entities at asserted c
onnectivities');
#32283=UNCERTAINTY_MEASURE_WITH_UNIT(LENGTH_MEASURE(0.01),#32310,
'DISTANCE_ACCURACY_VALUE',
'Maximum model space distance between geometric entities at asserted c
onnectivities');
#32284=UNCERTAINTY_MEASURE_WITH_UNIT(LENGTH_MEASURE(0.01),#32310,
'DISTANCE_ACCURACY_VALUE',
'Maximum model space distance between geometric entities at asserted c
onnectivities');
#32285=UNCERTAINTY_MEASURE_WITH_UNIT(LENGTH_MEASURE(0.01),#32310,
'DISTANCE_ACCURACY_VALUE',
'Maximum model space distance between geometric entities at asserted c
onnectivities');
#32286=UNCERTAINTY_MEASURE_WITH_UNIT(LENGTH_MEASURE(0.01),#32310,
'DISTANCE_ACCURACY_VALUE',
'Maximum model space distance between geometric entities at asserted c
onnectivities');
#32287=UNCERTAINTY_MEASURE_WITH_UNIT(LENGTH_MEASURE(0.01),#32310,
'DISTANCE_ACCURACY_VALUE',
'Maximum model space distance between geometric entities at asserted c
onnectivities');
#32288=UNCERTAINTY_MEASURE_WITH_UNIT(LENGTH_MEASURE(0.01),#32310,
'DISTANCE_ACCURACY_VALUE',
'Maximum model space distance between geometric entities at asserted c
onnectivities');
#32289=UNCERTAINTY_MEASURE_WITH_UNIT(LENGTH_MEASURE(0.01),#32310,
'DISTANCE_ACCURACY_VALUE',
'Maximum model space distance between geometric entities at asserted c
onnectivities');
#32290=UNCERTAINTY_MEASURE_WITH_UNIT(LENGTH_MEASURE(0.01),#32310,
'DISTANCE_ACCURACY_VALUE',
'Maximum model space distance between geometric entities at asserted c
onnectivities');
#32291=UNCERTAINTY_MEASURE_WITH_UNIT(LENGTH_MEASURE(0.01),#32310,
'DISTANCE_ACCURACY_VALUE',
'Maximum model space distance between geometric entities at asserted c
onnectivities');
#32292=UNCERTAINTY_MEASURE_WITH_UNIT(LENGTH_MEASURE(0.01),#32310,
'DISTANCE_ACCURACY_VALUE',
'Maximum model space distance between geometric entities at asserted c
onnectivities');
#32293=UNCERTAINTY_MEASURE_WITH_UNIT(LENGTH_MEASURE(0.01),#32310,
'DISTANCE_ACCURACY_VALUE',
'Maximum model space distance between geometric entities at asserted c
onnectivities');
#32294=(
GEOMETRIC_REPRESENTATION_CONTEXT(3)
GLOBAL_UNCERTAINTY_ASSIGNED_CONTEXT((#32278))
GLOBAL_UNIT_ASSIGNED_CONTEXT((#32310,#32312,#32313))
REPRESENTATION_CONTEXT('','3D')
);
#32295=(
GEOMETRIC_REPRESENTATION_CONTEXT(3)
GLOBAL_UNCERTAINTY_ASSIGNED_CONTEXT((#32279))
GLOBAL_UNIT_ASSIGNED_CONTEXT((#32310,#32312,#32313))
REPRESENTATION_CONTEXT('','3D')
);
#32296=(
GEOMETRIC_REPRESENTATION_CONTEXT(3)
GLOBAL_UNCERTAINTY_ASSIGNED_CONTEXT((#32280))
GLOBAL_UNIT_ASSIGNED_CONTEXT((#32310,#32312,#32313))
REPRESENTATION_CONTEXT('','3D')
);
#32297=(
GEOMETRIC_REPRESENTATION_CONTEXT(3)
GLOBAL_UNCERTAINTY_ASSIGNED_CONTEXT((#32281))
GLOBAL_UNIT_ASSIGNED_CONTEXT((#32310,#32312,#32313))
REPRESENTATION_CONTEXT('','3D')
);
#32298=(
GEOMETRIC_REPRESENTATION_CONTEXT(3)
GLOBAL_UNCERTAINTY_ASSIGNED_CONTEXT((#32282))
GLOBAL_UNIT_ASSIGNED_CONTEXT((#32310,#32312,#32313))
REPRESENTATION_CONTEXT('','3D')
);
#32299=(
GEOMETRIC_REPRESENTATION_CONTEXT(3)
GLOBAL_UNCERTAINTY_ASSIGNED_CONTEXT((#32283))
GLOBAL_UNIT_ASSIGNED_CONTEXT((#32310,#32312,#32313))
REPRESENTATION_CONTEXT('','3D')
);
#32300=(
GEOMETRIC_REPRESENTATION_CONTEXT(3)
GLOBAL_UNCERTAINTY_ASSIGNED_CONTEXT((#32284))
GLOBAL_UNIT_ASSIGNED_CONTEXT((#32310,#32312,#32313))
REPRESENTATION_CONTEXT('','3D')
);
#32301=(
GEOMETRIC_REPRESENTATION_CONTEXT(3)
GLOBAL_UNCERTAINTY_ASSIGNED_CONTEXT((#32285))
GLOBAL_UNIT_ASSIGNED_CONTEXT((#32310,#32312,#32313))
REPRESENTATION_CONTEXT('','3D')
);
#32302=(
GEOMETRIC_REPRESENTATION_CONTEXT(3)
GLOBAL_UNCERTAINTY_ASSIGNED_CONTEXT((#32286))
GLOBAL_UNIT_ASSIGNED_CONTEXT((#32310,#32312,#32313))
REPRESENTATION_CONTEXT('','3D')
);
#32303=(
GEOMETRIC_REPRESENTATION_CONTEXT(3)
GLOBAL_UNCERTAINTY_ASSIGNED_CONTEXT((#32287))
GLOBAL_UNIT_ASSIGNED_CONTEXT((#32310,#32312,#32313))
REPRESENTATION_CONTEXT('','3D')
);
#32304=(
GEOMETRIC_REPRESENTATION_CONTEXT(3)
GLOBAL_UNCERTAINTY_ASSIGNED_CONTEXT((#32288))
GLOBAL_UNIT_ASSIGNED_CONTEXT((#32310,#32312,#32313))
REPRESENTATION_CONTEXT('','3D')
);
#32305=(
GEOMETRIC_REPRESENTATION_CONTEXT(3)
GLOBAL_UNCERTAINTY_ASSIGNED_CONTEXT((#32289))
GLOBAL_UNIT_ASSIGNED_CONTEXT((#32310,#32312,#32313))
REPRESENTATION_CONTEXT('','3D')
);
#32306=(
GEOMETRIC_REPRESENTATION_CONTEXT(3)
GLOBAL_UNCERTAINTY_ASSIGNED_CONTEXT((#32290))
GLOBAL_UNIT_ASSIGNED_CONTEXT((#32310,#32312,#32313))
REPRESENTATION_CONTEXT('','3D')
);
#32307=(
GEOMETRIC_REPRESENTATION_CONTEXT(3)
GLOBAL_UNCERTAINTY_ASSIGNED_CONTEXT((#32291))
GLOBAL_UNIT_ASSIGNED_CONTEXT((#32310,#32312,#32313))
REPRESENTATION_CONTEXT('','3D')
);
#32308=(
GEOMETRIC_REPRESENTATION_CONTEXT(3)
GLOBAL_UNCERTAINTY_ASSIGNED_CONTEXT((#32292))
GLOBAL_UNIT_ASSIGNED_CONTEXT((#32310,#32312,#32313))
REPRESENTATION_CONTEXT('','3D')
);
#32309=(
GEOMETRIC_REPRESENTATION_CONTEXT(3)
GLOBAL_UNCERTAINTY_ASSIGNED_CONTEXT((#32293))
GLOBAL_UNIT_ASSIGNED_CONTEXT((#32310,#32312,#32313))
REPRESENTATION_CONTEXT('','3D')
);
#32310=(
LENGTH_UNIT()
NAMED_UNIT(*)
SI_UNIT(.MILLI.,.METRE.)
);
#32311=(
LENGTH_UNIT()
NAMED_UNIT(*)
SI_UNIT($,.METRE.)
);
#32312=(
NAMED_UNIT(*)
PLANE_ANGLE_UNIT()
SI_UNIT($,.RADIAN.)
);
#32313=(
NAMED_UNIT(*)
SI_UNIT($,.STERADIAN.)
SOLID_ANGLE_UNIT()
);
#32314=SHAPE_DEFINITION_REPRESENTATION(#32329,#32361);
#32315=SHAPE_DEFINITION_REPRESENTATION(#32330,#32362);
#32316=SHAPE_DEFINITION_REPRESENTATION(#32331,#32363);
#32317=SHAPE_DEFINITION_REPRESENTATION(#32332,#32364);
#32318=SHAPE_DEFINITION_REPRESENTATION(#32333,#32365);
#32319=SHAPE_DEFINITION_REPRESENTATION(#32334,#32366);
#32320=SHAPE_DEFINITION_REPRESENTATION(#32335,#32367);
#32321=SHAPE_DEFINITION_REPRESENTATION(#32336,#32368);
#32322=SHAPE_DEFINITION_REPRESENTATION(#32337,#32369);
#32323=SHAPE_DEFINITION_REPRESENTATION(#32338,#32370);
#32324=SHAPE_DEFINITION_REPRESENTATION(#32339,#32371);
#32325=SHAPE_DEFINITION_REPRESENTATION(#32340,#32372);
#32326=SHAPE_DEFINITION_REPRESENTATION(#32341,#32373);
#32327=SHAPE_DEFINITION_REPRESENTATION(#32342,#32374);
#32328=SHAPE_DEFINITION_REPRESENTATION(#32343,#32375);
#32329=PRODUCT_DEFINITION_SHAPE('',$,#32377);
#32330=PRODUCT_DEFINITION_SHAPE('',$,#32378);
#32331=PRODUCT_DEFINITION_SHAPE('',$,#32379);
#32332=PRODUCT_DEFINITION_SHAPE('',$,#32380);
#32333=PRODUCT_DEFINITION_SHAPE('',$,#32381);
#32334=PRODUCT_DEFINITION_SHAPE('',$,#32382);
#32335=PRODUCT_DEFINITION_SHAPE('',$,#32383);
#32336=PRODUCT_DEFINITION_SHAPE('',$,#32384);
#32337=PRODUCT_DEFINITION_SHAPE('',$,#32385);
#32338=PRODUCT_DEFINITION_SHAPE('',$,#32386);
#32339=PRODUCT_DEFINITION_SHAPE('',$,#32387);
#32340=PRODUCT_DEFINITION_SHAPE('',$,#32388);
#32341=PRODUCT_DEFINITION_SHAPE('',$,#32389);
#32342=PRODUCT_DEFINITION_SHAPE('',$,#32390);
#32343=PRODUCT_DEFINITION_SHAPE('',$,#32391);
#32344=PRODUCT_DEFINITION_SHAPE($,$,#62);
#32345=PRODUCT_DEFINITION_SHAPE($,$,#63);
#32346=PRODUCT_DEFINITION_SHAPE($,$,#64);
#32347=PRODUCT_DEFINITION_SHAPE($,$,#65);
#32348=PRODUCT_DEFINITION_SHAPE($,$,#66);
#32349=PRODUCT_DEFINITION_SHAPE($,$,#67);
#32350=PRODUCT_DEFINITION_SHAPE($,$,#68);
#32351=PRODUCT_DEFINITION_SHAPE($,$,#69);
#32352=PRODUCT_DEFINITION_SHAPE($,$,#70);
#32353=PRODUCT_DEFINITION_SHAPE($,$,#71);
#32354=PRODUCT_DEFINITION_SHAPE($,$,#72);
#32355=PRODUCT_DEFINITION_SHAPE($,$,#73);
#32356=PRODUCT_DEFINITION_SHAPE($,$,#74);
#32357=PRODUCT_DEFINITION_SHAPE($,$,#75);
#32358=PRODUCT_DEFINITION_SHAPE($,$,#76);
#32359=PRODUCT_DEFINITION_SHAPE($,$,#77);
#32360=PRODUCT_DEFINITION_SHAPE($,$,#78);
#32361=SHAPE_REPRESENTATION('',(#13973,#14987,#14988,#14989,#14990,#14991,
#14992,#14993,#14994,#14995,#14996,#14997,#14998,#14999,#15000,#15001,#15002,
#15003),#32294);
#32362=SHAPE_REPRESENTATION('',(#13974),#32295);
#32363=SHAPE_REPRESENTATION('',(#14060),#32296);
#32364=SHAPE_REPRESENTATION('',(#14095),#32297);
#32365=SHAPE_REPRESENTATION('',(#14114),#32298);
#32366=SHAPE_REPRESENTATION('',(#14204),#32299);
#32367=SHAPE_REPRESENTATION('',(#14378),#32300);
#32368=SHAPE_REPRESENTATION('',(#14413),#32301);
#32369=SHAPE_REPRESENTATION('',(#14432),#32302);
#32370=SHAPE_REPRESENTATION('',(#14610),#32303);
#32371=SHAPE_REPRESENTATION('',(#14627),#32304);
#32372=SHAPE_REPRESENTATION('',(#14637),#32305);
#32373=SHAPE_REPRESENTATION('',(#14690),#32306);
#32374=SHAPE_REPRESENTATION('',(#14802),#32307);
#32375=SHAPE_REPRESENTATION('',(#14889),#32308);
#32376=PRODUCT_DEFINITION_CONTEXT('part definition',#32423,'design');
#32377=PRODUCT_DEFINITION('2026-10-25-00-35-14-557','MAS-499',#32392,#32376);
#32378=PRODUCT_DEFINITION('2026-10-25-00-35-15-561',
'01_Outer_Tube_2.5sq_x_3-16',#32393,#32376);
#32379=PRODUCT_DEFINITION('2026-10-25-00-35-15-886',
'02_Outer_End_Plate_6in',#32394,#32376);
#32380=PRODUCT_DEFINITION('2026-10-25-00-35-16-091',
'03_Outer_Door_Plate_3in',#32395,#32376);
#32381=PRODUCT_DEFINITION('2026-10-25-00-35-16-238',
'04_Lock_Receiver_1.75sq',#32396,#32376);
#32382=PRODUCT_DEFINITION('2026-10-25-00-35-16-655',
'05_Inner_Tube_2sq_x_3-16_Lock_Holes',#32397,#32376);
#32383=PRODUCT_DEFINITION('2026-10-25-00-35-17-554',
'06_Inner_End_Plate_6in',#32398,#32376);
#32384=PRODUCT_DEFINITION('2026-10-25-00-35-17-868',
'07_Inner_Door_Plate_3in',#32399,#32376);
#32385=PRODUCT_DEFINITION('2026-10-25-00-35-18-111',
'08_Combination_Barrel_Lock_Body',#32400,#32376);
#32386=PRODUCT_DEFINITION('2026-10-25-00-35-19-682',
'09_Lock_Plunger_3-8',#32401,#32376);
#32387=PRODUCT_DEFINITION('2026-10-25-00-35-20-536',
'11_Dial_Axle_Pin_3x39',#32402,#32376);
#32388=PRODUCT_DEFINITION('2026-10-25-00-35-20-799',
'12_Spring_Pin_ISO_8752_4.76x12',#32403,#32376);
#32389=PRODUCT_DEFINITION('2026-10-25-00-35-21-990',
'13_Rubber_Lock_Boot',#32404,#32376);
#32390=PRODUCT_DEFINITION('2026-10-25-00-35-23-176',
'14_Tethered_Dust_Cap',#32405,#32376);
#32391=PRODUCT_DEFINITION('2026-10-25-00-35-19-921',
'10_Combination_Dial_Wheel',#32406,#32376);
#32392=PRODUCT_DEFINITION_FORMATION('',$,#32425);
#32393=PRODUCT_DEFINITION_FORMATION('',$,#32426);
#32394=PRODUCT_DEFINITION_FORMATION('',$,#32427);
#32395=PRODUCT_DEFINITION_FORMATION('',$,#32428);
#32396=PRODUCT_DEFINITION_FORMATION('',$,#32429);
#32397=PRODUCT_DEFINITION_FORMATION('',$,#32430);
#32398=PRODUCT_DEFINITION_FORMATION('',$,#32431);
#32399=PRODUCT_DEFINITION_FORMATION('',$,#32432);
#32400=PRODUCT_DEFINITION_FORMATION('',$,#32433);
#32401=PRODUCT_DEFINITION_FORMATION('',$,#32434);
#32402=PRODUCT_DEFINITION_FORMATION('',$,#32435);
#32403=PRODUCT_DEFINITION_FORMATION('',$,#32436);
#32404=PRODUCT_DEFINITION_FORMATION('',$,#32437);
#32405=PRODUCT_DEFINITION_FORMATION('',$,#32438);
#32406=PRODUCT_DEFINITION_FORMATION('',$,#32439);
#32407=PRODUCT_RELATED_PRODUCT_CATEGORY('MAS-499','MAS-499',(#32425));
#32408=PRODUCT_RELATED_PRODUCT_CATEGORY('01_Outer_Tube_2.5sq_x_3-16',
'01_Outer_Tube_2.5sq_x_3-16',(#32426));
#32409=PRODUCT_RELATED_PRODUCT_CATEGORY('02_Outer_End_Plate_6in',
'02_Outer_End_Plate_6in',(#32427));
#32410=PRODUCT_RELATED_PRODUCT_CATEGORY('03_Outer_Door_Plate_3in',
'03_Outer_Door_Plate_3in',(#32428));
#32411=PRODUCT_RELATED_PRODUCT_CATEGORY('04_Lock_Receiver_1.75sq',
'04_Lock_Receiver_1.75sq',(#32429));
#32412=PRODUCT_RELATED_PRODUCT_CATEGORY(
'05_Inner_Tube_2sq_x_3-16_Lock_Holes',
'05_Inner_Tube_2sq_x_3-16_Lock_Holes',(#32430));
#32413=PRODUCT_RELATED_PRODUCT_CATEGORY('06_Inner_End_Plate_6in',
'06_Inner_End_Plate_6in',(#32431));
#32414=PRODUCT_RELATED_PRODUCT_CATEGORY('07_Inner_Door_Plate_3in',
'07_Inner_Door_Plate_3in',(#32432));
#32415=PRODUCT_RELATED_PRODUCT_CATEGORY(
'08_Combination_Barrel_Lock_Body','08_Combination_Barrel_Lock_Body',(#32433));
#32416=PRODUCT_RELATED_PRODUCT_CATEGORY('09_Lock_Plunger_3-8',
'09_Lock_Plunger_3-8',(#32434));
#32417=PRODUCT_RELATED_PRODUCT_CATEGORY('11_Dial_Axle_Pin_3x39',
'11_Dial_Axle_Pin_3x39',(#32435));
#32418=PRODUCT_RELATED_PRODUCT_CATEGORY(
'12_Spring_Pin_ISO_8752_4.76x12','12_Spring_Pin_ISO_8752_4.76x12',(#32436));
#32419=PRODUCT_RELATED_PRODUCT_CATEGORY('13_Rubber_Lock_Boot',
'13_Rubber_Lock_Boot',(#32437));
#32420=PRODUCT_RELATED_PRODUCT_CATEGORY('14_Tethered_Dust_Cap',
'14_Tethered_Dust_Cap',(#32438));
#32421=PRODUCT_RELATED_PRODUCT_CATEGORY('10_Combination_Dial_Wheel',
'10_Combination_Dial_Wheel',(#32439));
#32422=APPLICATION_PROTOCOL_DEFINITION('international standard',
'automotive_design',2009,#32423);
#32423=APPLICATION_CONTEXT(
'Core Data for Automotive Mechanical Design Process');
#32424=PRODUCT_CONTEXT('part definition',#32423,'mechanical');
#32425=PRODUCT('2026-10-25-00-35-14-557','MAS-499',$,(#32424));
#32426=PRODUCT('2026-10-25-00-35-15-561','01_Outer_Tube_2.5sq_x_3-16',$,
(#32424));
#32427=PRODUCT('2026-10-25-00-35-15-886','02_Outer_End_Plate_6in',$,(#32424));
#32428=PRODUCT('2026-10-25-00-35-16-091','03_Outer_Door_Plate_3in',$,(#32424));
#32429=PRODUCT('2026-10-25-00-35-16-238','04_Lock_Receiver_1.75sq',$,(#32424));
#32430=PRODUCT('2026-10-25-00-35-16-655',
'05_Inner_Tube_2sq_x_3-16_Lock_Holes',$,(#32424));
#32431=PRODUCT('2026-10-25-00-35-17-554','06_Inner_End_Plate_6in',$,(#32424));
#32432=PRODUCT('2026-10-25-00-35-17-868','07_Inner_Door_Plate_3in',$,(#32424));
#32433=PRODUCT('2026-10-25-00-35-18-111',
'08_Combination_Barrel_Lock_Body',$,(#32424));
#32434=PRODUCT('2026-10-25-00-35-19-682','09_Lock_Plunger_3-8',$,(#32424));
#32435=PRODUCT('2026-10-25-00-35-20-536','11_Dial_Axle_Pin_3x39',$,(#32424));
#32436=PRODUCT('2026-10-25-00-35-20-799',
'12_Spring_Pin_ISO_8752_4.76x12',$,(#32424));
#32437=PRODUCT('2026-10-25-00-35-21-990','13_Rubber_Lock_Boot',$,(#32424));
#32438=PRODUCT('2026-10-25-00-35-23-176','14_Tethered_Dust_Cap',$,(#32424));
#32439=PRODUCT('2026-10-25-00-35-19-921','10_Combination_Dial_Wheel',$,
(#32424));
#32440=PRESENTATION_STYLE_ASSIGNMENT((#32445));
#32441=PRESENTATION_STYLE_ASSIGNMENT((#32446));
#32442=PRESENTATION_STYLE_ASSIGNMENT((#32447));
#32443=PRESENTATION_STYLE_ASSIGNMENT((#32448));
#32444=PRESENTATION_STYLE_ASSIGNMENT((#32449));
#32445=SURFACE_STYLE_USAGE(.BOTH.,#32450);
#32446=SURFACE_STYLE_USAGE(.BOTH.,#32451);
#32447=SURFACE_STYLE_USAGE(.BOTH.,#32452);
#32448=SURFACE_STYLE_USAGE(.BOTH.,#32453);
#32449=SURFACE_STYLE_USAGE(.BOTH.,#32454);
#32450=SURFACE_SIDE_STYLE('',(#32455));
#32451=SURFACE_SIDE_STYLE('',(#32456));
#32452=SURFACE_SIDE_STYLE('',(#32457));
#32453=SURFACE_SIDE_STYLE('',(#32458));
#32454=SURFACE_SIDE_STYLE('',(#32459));
#32455=SURFACE_STYLE_FILL_AREA(#32460);
#32456=SURFACE_STYLE_FILL_AREA(#32461);
#32457=SURFACE_STYLE_FILL_AREA(#32462);
#32458=SURFACE_STYLE_FILL_AREA(#32463);
#32459=SURFACE_STYLE_FILL_AREA(#32464);
#32460=FILL_AREA_STYLE('Steel - Satin',(#32465));
#32461=FILL_AREA_STYLE('MAS496_al',(#32466));
#32462=FILL_AREA_STYLE('MAS496_ti',(#32467));
#32463=FILL_AREA_STYLE('MAS496_ss',(#32468));
#32464=FILL_AREA_STYLE('MAS496_gun',(#32469));
#32465=FILL_AREA_STYLE_COLOUR('Steel - Satin',#32470);
#32466=FILL_AREA_STYLE_COLOUR('MAS496_al',#32471);
#32467=FILL_AREA_STYLE_COLOUR('MAS496_ti',#32472);
#32468=FILL_AREA_STYLE_COLOUR('MAS496_ss',#32473);
#32469=FILL_AREA_STYLE_COLOUR('MAS496_gun',#32474);
#32470=COLOUR_RGB('Steel - Satin',0.627450980392157,0.627450980392157,0.627450980392157);
#32471=COLOUR_RGB('MAS496_al',0.67843137254902,0.705882352941177,0.729411764705882);
#32472=COLOUR_RGB('MAS496_ti',0.549019607843137,0.572549019607843,0.596078431372549);
#32473=COLOUR_RGB('MAS496_ss',0.83921568627451,0.850980392156863,0.862745098039216);
#32474=COLOUR_RGB('MAS496_gun',0.313725490196078,0.337254901960784,0.364705882352941);
#32475=COLOUR_RGB('Dark Blue',0.08,0.2,0.34);
#32476=FILL_AREA_STYLE_COLOUR('',#32475);
#32477=FILL_AREA_STYLE('',(#32476));
#32478=SURFACE_STYLE_FILL_AREA(#32477);
#32479=SURFACE_SIDE_STYLE('',(#32478));
#32480=SURFACE_STYLE_USAGE(.BOTH.,#32479);
#32481=PRESENTATION_STYLE_ASSIGNMENT((#32480));
#32482=COLOUR_RGB('Light Blue',0.38,0.62,0.78);
#32483=FILL_AREA_STYLE_COLOUR('',#32482);
#32484=FILL_AREA_STYLE('',(#32483));
#32485=SURFACE_STYLE_FILL_AREA(#32484);
#32486=SURFACE_SIDE_STYLE('',(#32485));
#32487=SURFACE_STYLE_USAGE(.BOTH.,#32486);
#32488=PRESENTATION_STYLE_ASSIGNMENT((#32487));
#32489=COLOUR_RGB('Sky Blue',0.24,0.69,0.87);
#32490=FILL_AREA_STYLE_COLOUR('',#32489);
#32491=FILL_AREA_STYLE('',(#32490));
#32492=SURFACE_STYLE_FILL_AREA(#32491);
#32493=SURFACE_SIDE_STYLE('',(#32492));
#32494=SURFACE_STYLE_USAGE(.BOTH.,#32493);
#32495=PRESENTATION_STYLE_ASSIGNMENT((#32494));
#32496=COLOUR_RGB('Grey',0.48,0.52,0.57);
#32497=FILL_AREA_STYLE_COLOUR('',#32496);
#32498=FILL_AREA_STYLE('',(#32497));
#32499=SURFACE_STYLE_FILL_AREA(#32498);
#32500=SURFACE_SIDE_STYLE('',(#32499));
#32501=SURFACE_STYLE_USAGE(.BOTH.,#32500);
#32502=PRESENTATION_STYLE_ASSIGNMENT((#32501));
#32503=COLOUR_RGB('Black',0.12,0.14,0.17);
#32504=FILL_AREA_STYLE_COLOUR('',#32503);
#32505=FILL_AREA_STYLE('',(#32504));
#32506=SURFACE_STYLE_FILL_AREA(#32505);
#32507=SURFACE_SIDE_STYLE('',(#32506));
#32508=SURFACE_STYLE_USAGE(.BOTH.,#32507);
#32509=PRESENTATION_STYLE_ASSIGNMENT((#32508));
#32510=COLOUR_RGB('Off White',0.89,0.88,0.83);
#32511=FILL_AREA_STYLE_COLOUR('',#32510);
#32512=FILL_AREA_STYLE('',(#32511));
#32513=SURFACE_STYLE_FILL_AREA(#32512);
#32514=SURFACE_SIDE_STYLE('',(#32513));
#32515=SURFACE_STYLE_USAGE(.BOTH.,#32514);
#32516=PRESENTATION_STYLE_ASSIGNMENT((#32515));
ENDSEC;
END-ISO-10303-21;
